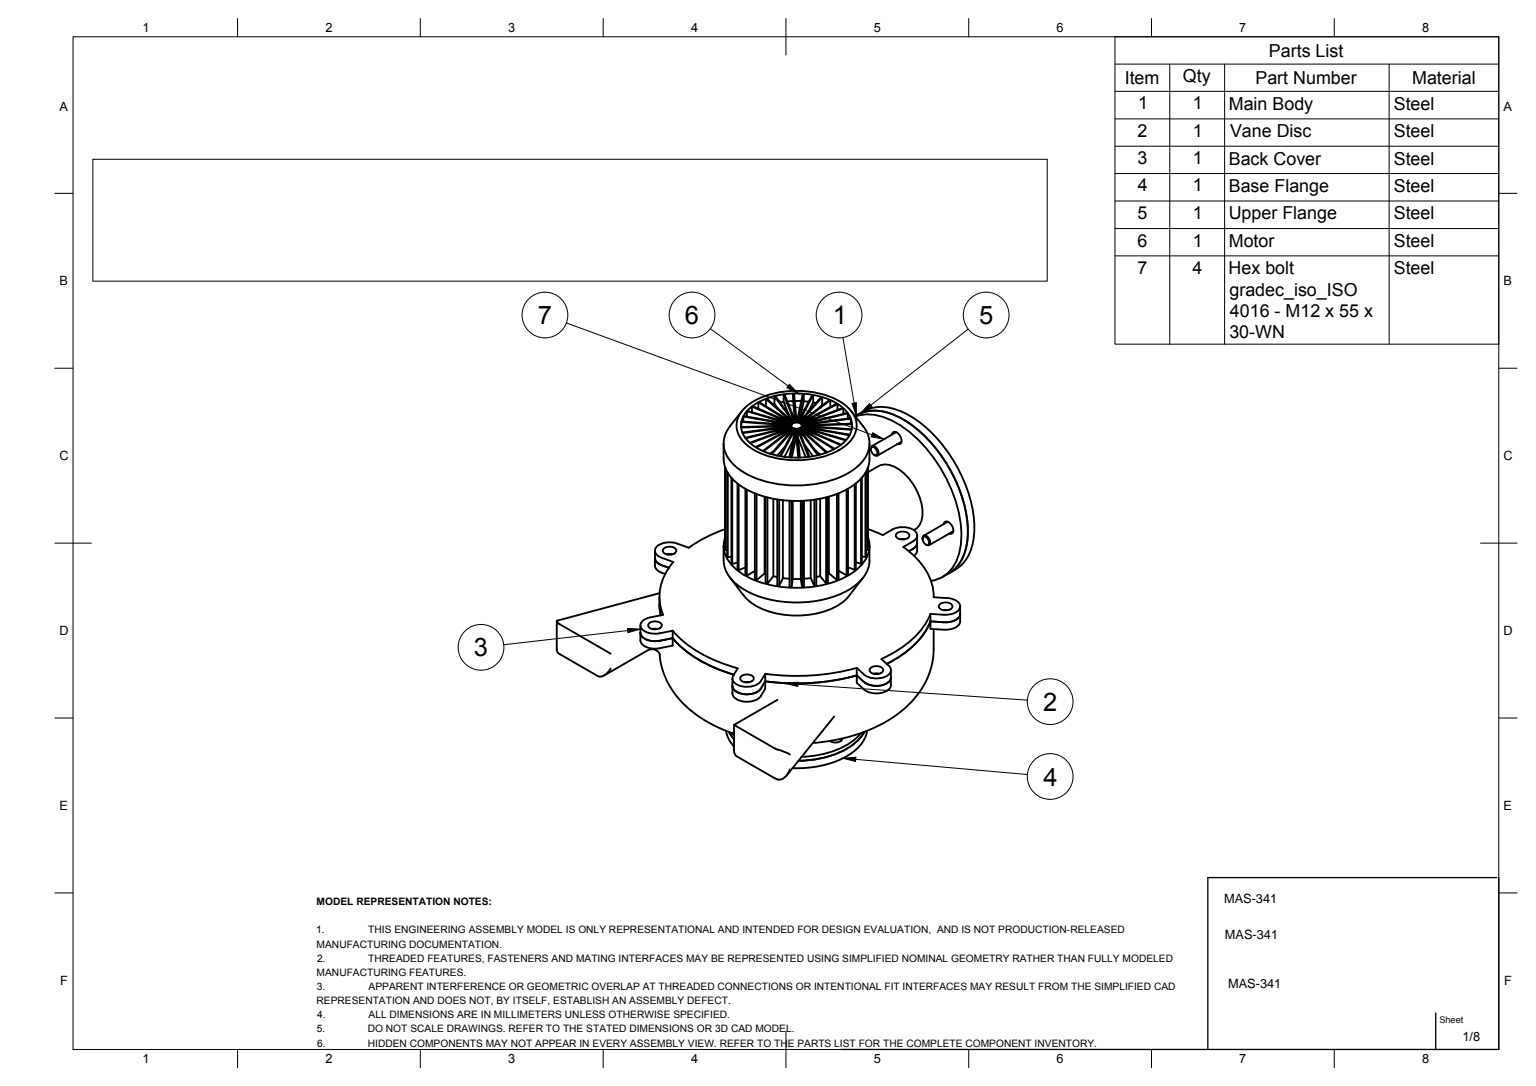
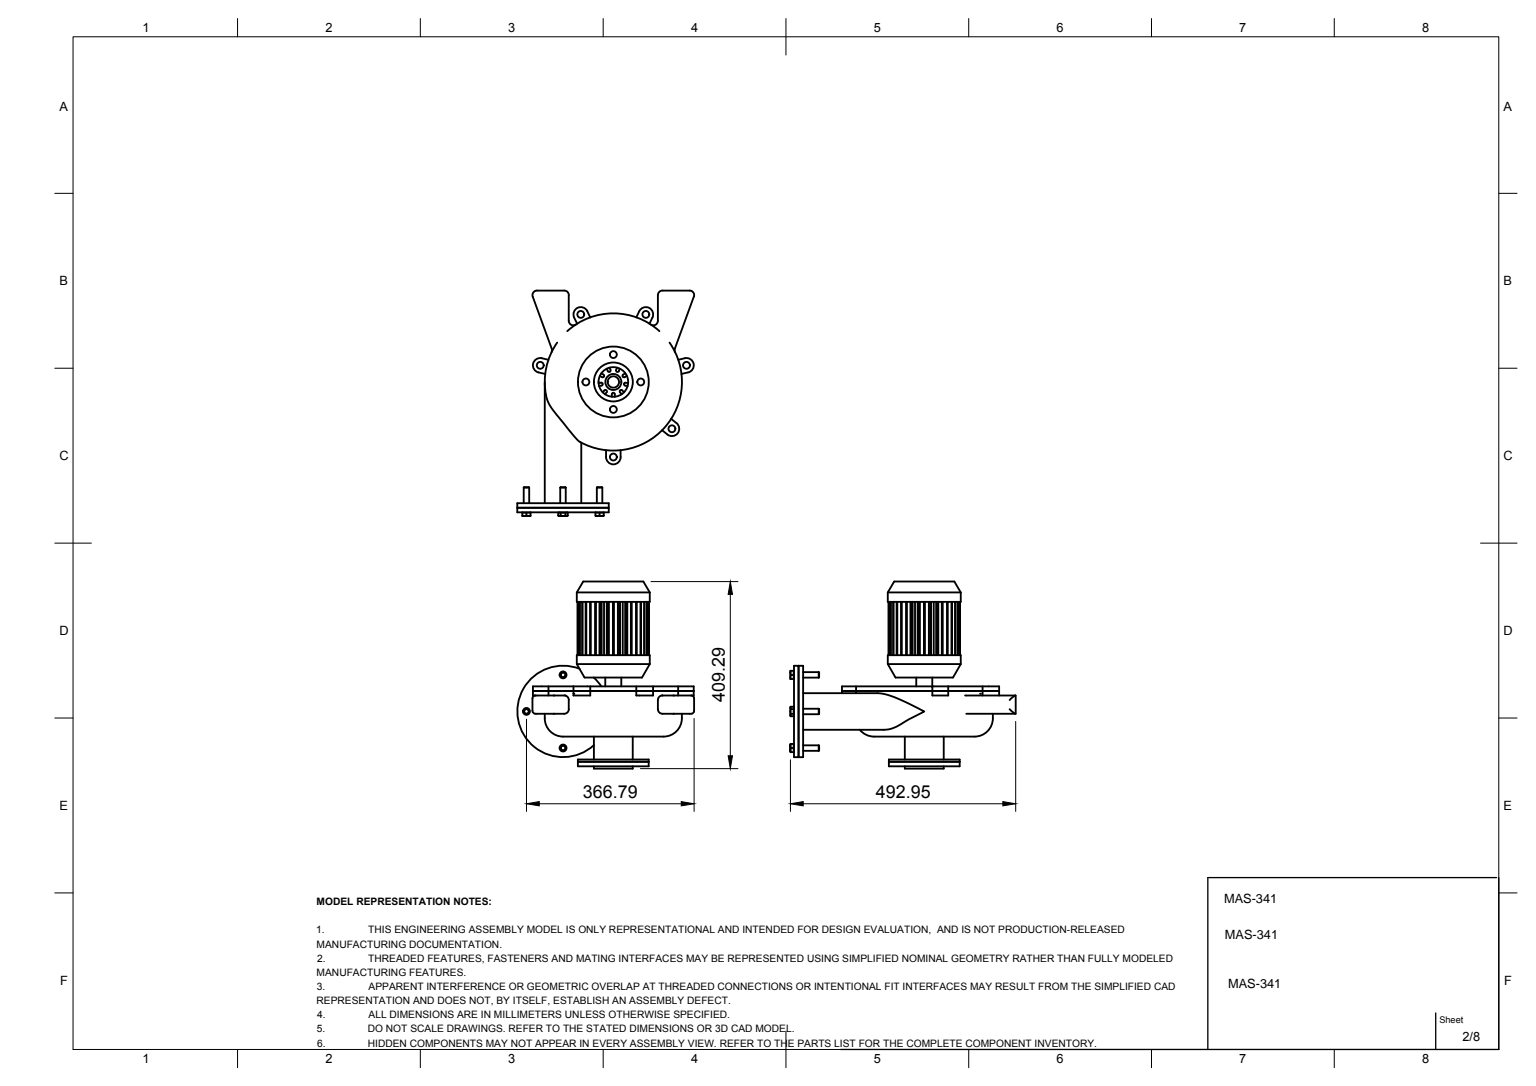
ISO-10303-21;
HEADER;
FILE_DESCRIPTION (('STEP AP214'),
    '1' );
FILE_NAME ('MAS-341',
    '2026-10-08T00:39:10',
    ( '' ),
    ( '' ),
    'SwSTEP 2.0',
    'SolidWorks 2025',
    '' );
FILE_SCHEMA (( 'AUTOMOTIVE_DESIGN' ));
ENDSEC;

DATA;
#1 = VERTEX_POINT ( 'NONE', #4469 ) ;
#2 = CARTESIAN_POINT ( 'NONE',  ( 97.60910239587762760, -133.8115172545202540, 8.514989709614523505 ) ) ;
#3 = DIRECTION ( 'NONE',  ( 0.000000000000000000, 0.000000000000000000, 1.000000000000000000 ) ) ;
#4 = PRODUCT ( 'Back Cover', 'Back Cover', '', ( #531 ) ) ;
#5 = EDGE_CURVE ( 'NONE', #5734, #13358, #17540, .T. ) ;
#6 = EDGE_CURVE ( 'NONE', #9325, #3604, #16957, .T. ) ;
#7 = DIRECTION ( 'NONE',  ( 0.000000000000000000, 0.000000000000000000, 1.000000000000000000 ) ) ;
#8 = AXIS2_PLACEMENT_3D ( 'NONE', #20241, #7754, #6443 ) ;
#9 = CARTESIAN_POINT ( 'NONE',  ( 0.000000000000000000, 0.000000000000000000, 49.99999999999999289 ) ) ;
#10 = VERTEX_POINT ( 'NONE', #9173 ) ;
#11 = LINE ( 'NONE', #3084, #15099 ) ;
#12 =( GEOMETRIC_REPRESENTATION_CONTEXT ( 3 ) GLOBAL_UNCERTAINTY_ASSIGNED_CONTEXT ( ( #1291 ) ) GLOBAL_UNIT_ASSIGNED_CONTEXT ( ( #18131, #16699, #13613 ) ) REPRESENTATION_CONTEXT ( 'NONE', 'WORKASPACE' ) );
#13 = DIRECTION ( 'NONE',  ( 1.000000000000000000, 0.000000000000000000, 0.000000000000000000 ) ) ;
#14 = CARTESIAN_POINT ( 'NONE',  ( 1.379293853801755176, -58.69016442926522359, 112.7772637782949943 ) ) ;
#15 = VECTOR ( 'NONE', #9741, 1000.000000000000000 ) ;
#16 = CARTESIAN_POINT ( 'NONE',  ( 95.93567628220807819, -116.0760901523964179, 30.45195958925782520 ) ) ;
#17 = VERTEX_POINT ( 'NONE', #1406 ) ;
#18 = LINE ( 'NONE', #19855, #18549 ) ;
#19 = CARTESIAN_POINT ( 'NONE',  ( -47.56244194535165803, -37.78198917157333625, 283.5832628385307999 ) ) ;
#20 = ORIENTED_EDGE ( 'NONE', *, *, #18426, .T. ) ;
#21 = ORIENTED_EDGE ( 'NONE', *, *, #3297, .T. ) ;
#22 = VERTEX_POINT ( 'NONE', #7636 ) ;
#23 = EDGE_CURVE ( 'NONE', #17780, #6819, #12333, .T. ) ;
#24 = DIRECTION ( 'NONE',  ( 1.000000000000000000, 0.000000000000000000, 0.000000000000000000 ) ) ;
#25 = ORIENTED_EDGE ( 'NONE', *, *, #13470, .F. ) ;
#26 = CARTESIAN_POINT ( 'NONE',  ( 78.68887634719571622, -147.8252249328912740, 39.99999999999999289 ) ) ;
#27 = FACE_BOUND ( 'NONE', #13868, .T. ) ;
#28 = ORIENTED_EDGE ( 'NONE', *, *, #7214, .F. ) ;
#29 = VECTOR ( 'NONE', #19093, 1000.000000000000000 ) ;
#30 = DIRECTION ( 'NONE',  ( 0.000000000000000000, 0.000000000000000000, 1.000000000000000000 ) ) ;
#31 = FACE_OUTER_BOUND ( 'NONE', #4493, .T. ) ;
#32 = CARTESIAN_POINT ( 'NONE',  ( 130.7934332354521132, -73.44669674648567081, 45.54261232719608188 ) ) ;
#33 = CARTESIAN_POINT ( 'NONE',  ( -84.44661573609343463, -123.9709896190455680, 39.82577217277482617 ) ) ;
#34 = EDGE_CURVE ( 'NONE', #17780, #13430, #14084, .T. ) ;
#35 = DIRECTION ( 'NONE',  ( -0.000000000000000000, -0.000000000000000000, 1.000000000000000000 ) ) ;
#36 = DIRECTION ( 'NONE',  ( 1.000000000000000000, 0.000000000000000000, 0.000000000000000000 ) ) ;
#37 = EDGE_CURVE ( 'NONE', #15836, #9172, #3251, .T. ) ;
#38 = CARTESIAN_POINT ( 'NONE',  ( -139.9569363493348249, 3.997132000652560802, 23.09995224052206453 ) ) ;
#39 = DIRECTION ( 'NONE',  ( 0.000000000000000000, 0.000000000000000000, 1.000000000000000000 ) ) ;
#40 = DIRECTION ( 'NONE',  ( -0.9396926207859104263, 0.3420201433256630508, 0.000000000000000000 ) ) ;
#41 = PLANE ( 'NONE',  #1345 ) ;
#42 = CARTESIAN_POINT ( 'NONE',  ( -133.8587666923834547, -78.85012038918891619, 37.00472930354037260 ) ) ;
#43 = ADVANCED_FACE ( 'NONE', ( #7739 ), #8149, .F. ) ;
#44 = ORIENTED_EDGE ( 'NONE', *, *, #7876, .F. ) ;
#45 = VECTOR ( 'NONE', #980, 1000.000000000000000 ) ;
#46 = DIRECTION ( 'NONE',  ( 0.000000000000000000, 1.000000000000000000, 0.000000000000000000 ) ) ;
#47 = AXIS2_PLACEMENT_3D ( 'NONE', #14477, #18892, #8730 ) ;
#48 = VERTEX_POINT ( 'NONE', #12848 ) ;
#49 = ORIENTED_EDGE ( 'NONE', *, *, #19031, .T. ) ;
#50 = ORIENTED_EDGE ( 'NONE', *, *, #6042, .F. ) ;
#51 = CARTESIAN_POINT ( 'NONE',  ( -144.9440567817290741, -14.18564734370175628, 2.776575249912347054 ) ) ;
#52 = CYLINDRICAL_SURFACE ( 'NONE', #15157, 62.91752772691707207 ) ;
#53 = CARTESIAN_POINT ( 'NONE',  ( 19.23677882349201695, -57.61823435390814296, 283.5832628385307999 ) ) ;
#54 = DIRECTION ( 'NONE',  ( -0.3747554100459959403, -0.9271237148521535021, 0.000000000000000000 ) ) ;
#55 = VERTEX_POINT ( 'NONE', #19106 ) ;
#56 = CARTESIAN_POINT ( 'NONE',  ( -95.11181282143326143, 95.73178764297979626, -26.71222966351301409 ) ) ;
#57 = CARTESIAN_POINT ( 'NONE',  ( -50.37374754117255549, -141.2886604036510221, 60.00000000000000000 ) ) ;
#58 = DIRECTION ( 'NONE',  ( -0.000000000000000000, -0.000000000000000000, -1.000000000000000000 ) ) ;
#59 = LINE ( 'NONE', #18583, #13084 ) ;
#60 = DIRECTION ( 'NONE',  ( -0.000000000000000000, -0.000000000000000000, 1.000000000000000000 ) ) ;
#61 = EDGE_CURVE ( 'NONE', #5572, #2811, #1813, .T. ) ;
#62 = ORIENTED_EDGE ( 'NONE', *, *, #6982, .T. ) ;
#63 = CARTESIAN_POINT ( 'NONE',  ( 134.0645693066686874, -77.56608579646832879, 36.26849213499117042 ) ) ;
#64 = CARTESIAN_POINT ( 'NONE',  ( -109.9999999999983515, 275.0000000000000000, 92.50000000000004263 ) ) ;
#65 = VERTEX_POINT ( 'NONE', #17476 ) ;
#66 = ORIENTED_EDGE ( 'NONE', *, *, #9551, .T. ) ;
#67 = ORIENTED_EDGE ( 'NONE', *, *, #294, .F. ) ;
#68 = ORIENTED_EDGE ( 'NONE', *, *, #8619, .T. ) ;
#69 = CARTESIAN_POINT ( 'NONE',  ( 57.41881860123199743, 83.27814316901175573, 14.88498244535504966 ) ) ;
#70 = VECTOR ( 'NONE', #7904, 1000.000000000000000 ) ;
#71 = ORIENTED_EDGE ( 'NONE', *, *, #11636, .F. ) ;
#72 = PLANE ( 'NONE',  #545 ) ;
#73 = DIRECTION ( 'NONE',  ( 1.000000000000000000, 0.000000000000000000, 0.000000000000000000 ) ) ;
#74 = DIRECTION ( 'NONE',  ( -0.000000000000000000, -0.000000000000000000, -1.000000000000000000 ) ) ;
#75 = LINE ( 'NONE', #4042, #2106 ) ;
#76 = CARTESIAN_POINT ( 'NONE',  ( 152.4599531637113330, -36.50981547336952104, 49.99999999999999289 ) ) ;
#77 = ORIENTED_EDGE ( 'NONE', *, *, #15533, .T. ) ;
#78 = DIRECTION ( 'NONE',  ( 0.4999999999999920619, -0.8660254037844431485, -3.488064225688951427E-15 ) ) ;
#79 = LINE ( 'NONE', #15635, #4891 ) ;
#80 = EDGE_LOOP ( 'NONE', ( #725, #12520, #18539, #7460 ) ) ;
#81 = UNCERTAINTY_MEASURE_WITH_UNIT (LENGTH_MEASURE( 1.000000000000000082E-05 ), #12072, 'distance_accuracy_value', 'NONE');
#82 = CARTESIAN_POINT ( 'NONE',  ( -82.22709333324932857, 122.5189358644918656, -23.80566512433226833 ) ) ;
#83 = CARTESIAN_POINT ( 'NONE',  ( -110.0000000000000142, 275.0000000000000000, 5.000000000000000888 ) ) ;
#84 = EDGE_CURVE ( 'NONE', #13974, #7495, #15567, .T. ) ;
#85 = CARTESIAN_POINT ( 'NONE',  ( 7.350000000000001421, 0.000000000000000000, 0.000000000000000000 ) ) ;
#86 = VECTOR ( 'NONE', #18456, 1000.000000000000000 ) ;
#87 = AXIS2_PLACEMENT_3D ( 'NONE', #5255, #2475, #14657 ) ;
#88 = LINE ( 'NONE', #6338, #12972 ) ;
#89 = CARTESIAN_POINT ( 'NONE',  ( 9.176097008933345123, -25.21111933077053990, 14.88498244535538895 ) ) ;
#90 = CARTESIAN_POINT ( 'NONE',  ( -56.84754764479025368, -154.7316448359455308, 49.99999999999999289 ) ) ;
#91 = ORIENTED_EDGE ( 'NONE', *, *, #10595, .F. ) ;
#92 = CARTESIAN_POINT ( 'NONE',  ( 128.2779226595531270, 102.2982297021113141, 60.00000000000000000 ) ) ;
#93 = VERTEX_POINT ( 'NONE', #12647 ) ;
#94 = VECTOR ( 'NONE', #4205, 1000.000000000000000 ) ;
#95 = ORIENTED_EDGE ( 'NONE', *, *, #17125, .F. ) ;
#96 = FACE_OUTER_BOUND ( 'NONE', #8145, .T. ) ;
#97 = EDGE_CURVE ( 'NONE', #13695, #10750, #5094, .T. ) ;
#98 = VERTEX_POINT ( 'NONE', #17267 ) ;
#99 = FACE_OUTER_BOUND ( 'NONE', #15672, .T. ) ;
#100 = FACE_BOUND ( 'NONE', #8738, .T. ) ;
#101 = ORIENTED_EDGE ( 'NONE', *, *, #14389, .F. ) ;
#102 = CARTESIAN_POINT ( 'NONE',  ( 100.3336596192663990, -130.0766330735003180, 3.023488127333376685 ) ) ;
#103 = CARTESIAN_POINT ( 'NONE',  ( 0.000000000000000000, 0.000000000000000000, 283.5832628385307999 ) ) ;
#104 = VECTOR ( 'NONE', #2637, 1000.000000000000000 ) ;
#105 = ADVANCED_FACE ( 'NONE', ( #15832 ), #1708, .T. ) ;
#106 = FACE_OUTER_BOUND ( 'NONE', #19908, .T. ) ;
#107 = SURFACE_SIDE_STYLE ('',( #15666 ) ) ;
#108 = VERTEX_POINT ( 'NONE', #3347 ) ;
#109 = CARTESIAN_POINT ( 'NONE',  ( 79.75827554147308263, 0.000000000000000000, 112.9440587442963562 ) ) ;
#110 = CYLINDRICAL_SURFACE ( 'NONE', #6774, 62.91752772691707207 ) ;
#111 = FACE_OUTER_BOUND ( 'NONE', #19672, .T. ) ;
#112 = CARTESIAN_POINT ( 'NONE',  ( 96.87131796860539623, -115.7364764686970489, 29.66028648393937317 ) ) ;
#113 = ORIENTED_EDGE ( 'NONE', *, *, #2779, .F. ) ;
#114 = DIRECTION ( 'NONE',  ( -3.129754055707530415E-16, 1.000000000000000000, 0.000000000000000000 ) ) ;
#115 = CARTESIAN_POINT ( 'NONE',  ( -70.46379820184749576, 132.4194400891323653, -1.343775461033565932 ) ) ;
#116 = AXIS2_PLACEMENT_3D ( 'NONE', #3572, #14207, #6645 ) ;
#117 = ORIENTED_EDGE ( 'NONE', *, *, #11334, .T. ) ;
#118 = EDGE_LOOP ( 'NONE', ( #19896, #4440, #15908, #1948 ) ) ;
#119 = ORIENTED_EDGE ( 'NONE', *, *, #13238, .T. ) ;
#120 =( NAMED_UNIT ( * ) SI_UNIT ( $, .STERADIAN. ) SOLID_ANGLE_UNIT ( ) );
#121 = EDGE_CURVE ( 'NONE', #7971, #3301, #6530, .T. ) ;
#122 = AXIS2_PLACEMENT_3D ( 'NONE', #14861, #16210, #14669 ) ;
#123 = EDGE_LOOP ( 'NONE', ( #19058, #8519, #18483, #4308 ) ) ;
#124 = ADVANCED_FACE ( 'NONE', ( #3050 ), #72, .T. ) ;
#125 = CARTESIAN_POINT ( 'NONE',  ( 28.06680738835026290, -53.87178215532764369, 293.5832628385307999 ) ) ;
#126 = LINE ( 'NONE', #5341, #13935 ) ;
#127 = VECTOR ( 'NONE', #6121, 1000.000000000000000 ) ;
#128 = ORIENTED_EDGE ( 'NONE', *, *, #9739, .T. ) ;
#129 = FACE_OUTER_BOUND ( 'NONE', #6146, .T. ) ;
#130 = DIRECTION ( 'NONE',  ( 0.000000000000000000, 1.000000000000000000, 0.000000000000000000 ) ) ;
#131 = DIRECTION ( 'NONE',  ( -0.1736481776669408228, -0.9848077530122062440, 2.152196535136390085E-15 ) ) ;
#132 = CARTESIAN_POINT ( 'NONE',  ( -95.59344839194261567, -116.1516065318577233, 31.25619608454541165 ) ) ;
#133 = LINE ( 'NONE', #6488, #17538 ) ;
#134 = CARTESIAN_POINT ( 'NONE',  ( -140.0000000000000284, 1.714505518806295230E-14, 23.02775637731986436 ) ) ;
#135 = EDGE_CURVE ( 'NONE', #17975, #14483, #10909, .T. ) ;
#136 = CARTESIAN_POINT ( 'NONE',  ( 141.8714406926368099, -48.70825716237082759, 49.99999999999999289 ) ) ;
#137 = VECTOR ( 'NONE', #8001, 1000.000000000000000 ) ;
#138 = CARTESIAN_POINT ( 'NONE',  ( -19.79297637435821500, 18.57624240429758800, 39.88498244535558968 ) ) ;
#139 = PLANE ( 'NONE',  #10813 ) ;
#140 = CARTESIAN_POINT ( 'NONE',  ( -123.8565975624213849, -84.62454961663081576, 40.61527585688936881 ) ) ;
#141 = VERTEX_POINT ( 'NONE', #14296 ) ;
#142 = DIRECTION ( 'NONE',  ( -0.000000000000000000, -0.000000000000000000, 1.000000000000000000 ) ) ;
#143 = CIRCLE ( 'NONE', #11572, 77.50000000000000000 ) ;
#144 = ORIENTED_EDGE ( 'NONE', *, *, #11299, .F. ) ;
#145 = EDGE_CURVE ( 'NONE', #10155, #5152, #9485, .T. ) ;
#146 = ADVANCED_FACE ( 'NONE', ( #6627 ), #17167, .F. ) ;
#147 = EDGE_LOOP ( 'NONE', ( #10880, #3979, #3844, #3785, #18936 ) ) ;
#148 = ADVANCED_FACE ( 'NONE', ( #7839 ), #6224, .F. ) ;
#149 = EDGE_CURVE ( 'NONE', #12149, #16123, #12294, .T. ) ;
#150 = ORIENTED_EDGE ( 'NONE', *, *, #14501, .F. ) ;
#151 = AXIS2_PLACEMENT_3D ( 'NONE', #5744, #3184, #10529 ) ;
#152 = CARTESIAN_POINT ( 'NONE',  ( -144.3459975433503359, -14.90824844061875432, 11.80575795572019437 ) ) ;
#153 = DIRECTION ( 'NONE',  ( 0.000000000000000000, 0.000000000000000000, -1.000000000000000000 ) ) ;
#154 = LINE ( 'NONE', #15601, #13008 ) ;
#155 = DIRECTION ( 'NONE',  ( 0.000000000000000000, 0.000000000000000000, 1.000000000000000000 ) ) ;
#156 = CARTESIAN_POINT ( 'NONE',  ( -77.50000000000000000, 9.491012693391988181E-15, -105.0000000000000142 ) ) ;
#157 = EDGE_CURVE ( 'NONE', #11944, #5361, #6437, .T. ) ;
#158 = LINE ( 'NONE', #9470, #15417 ) ;
#159 = DIRECTION ( 'NONE',  ( -0.000000000000000000, -0.000000000000000000, 1.000000000000000000 ) ) ;
#160 = CARTESIAN_POINT ( 'NONE',  ( 104.3997176008718668, -123.8500140569468897, 39.51069475786240304 ) ) ;
#161 = AXIS2_PLACEMENT_3D ( 'NONE', #19945, #4400, #6050 ) ;
#162 = CARTESIAN_POINT ( 'NONE',  ( 0.000000000000000000, 0.000000000000000000, 283.5832628385307999 ) ) ;
#163 = ORIENTED_EDGE ( 'NONE', *, *, #16525, .F. ) ;
#164 = CARTESIAN_POINT ( 'NONE',  ( 131.4393841463105730, -72.38802639019482399, 37.47509838629414247 ) ) ;
#165 = CARTESIAN_POINT ( 'NONE',  ( -97.49999999999997158, -195.8578643762690206, 4.142135623730952787 ) ) ;
#166 = VERTEX_POINT ( 'NONE', #19011 ) ;
#167 = ORIENTED_EDGE ( 'NONE', *, *, #19754, .F. ) ;
#168 = EDGE_CURVE ( 'NONE', #13542, #6667, #19206, .T. ) ;
#169 = ORIENTED_EDGE ( 'NONE', *, *, #10850, .T. ) ;
#170 = LINE ( 'NONE', #6528, #17757 ) ;
#171 = ORIENTED_EDGE ( 'NONE', *, *, #16914, .T. ) ;
#172 = CARTESIAN_POINT ( 'NONE',  ( 51.23821591265094355, 28.63313560863489471, 132.4711112102474146 ) ) ;
#173 = VECTOR ( 'NONE', #8479, 1000.000000000000000 ) ;
#174 = EDGE_CURVE ( 'NONE', #2962, #5478, #10345, .T. ) ;
#175 = DIRECTION ( 'NONE',  ( -0.000000000000000000, -0.000000000000000000, 1.000000000000000000 ) ) ;
#176 = FACE_BOUND ( 'NONE', #16626, .T. ) ;
#177 = CARTESIAN_POINT ( 'NONE',  ( 44.79940644582654841, -41.02350267428983699, 293.5832628385307999 ) ) ;
#178 = CARTESIAN_POINT ( 'NONE',  ( -85.53020504959707182, -140.9188050298390067, 49.99999999999999289 ) ) ;
#179 = ORIENTED_EDGE ( 'NONE', *, *, #8168, .F. ) ;
#180 = CARTESIAN_POINT ( 'NONE',  ( 125.6254798881099362, -81.96796683352708612, -9.529669441935290308 ) ) ;
#181 = CARTESIAN_POINT ( 'NONE',  ( -57.92514141135452377, -18.28503710798565152, 293.5832628385307999 ) ) ;
#182 = VERTEX_POINT ( 'NONE', #8245 ) ;
#183 = DIRECTION ( 'NONE',  ( -0.000000000000000000, -1.000000000000000000, -0.000000000000000000 ) ) ;
#184 = DIRECTION ( 'NONE',  ( -0.000000000000000000, -0.000000000000000000, 1.000000000000000000 ) ) ;
#185 = VECTOR ( 'NONE', #17338, 999.9999999999998863 ) ;
#186 = DIRECTION ( 'NONE',  ( 0.4999999999999978906, 0.8660254037844397068, 0.000000000000000000 ) ) ;
#187 = CYLINDRICAL_SURFACE ( 'NONE', #11980, 150.0000000000000284 ) ;
#188 =( GEOMETRIC_REPRESENTATION_CONTEXT ( 3 ) GLOBAL_UNCERTAINTY_ASSIGNED_CONTEXT ( ( #9055 ) ) GLOBAL_UNIT_ASSIGNED_CONTEXT ( ( #6659, #405, #9614 ) ) REPRESENTATION_CONTEXT ( 'NONE', 'WORKASPACE' ) );
#189 = CARTESIAN_POINT ( 'NONE',  ( 89.20186311087663000, -120.5960167300875980, 45.74363724982469392 ) ) ;
#190 = ORIENTED_EDGE ( 'NONE', *, *, #18942, .F. ) ;
#191 = CARTESIAN_POINT ( 'NONE',  ( -7.500000000000006217, 164.0736214083062805, 49.99999999999999289 ) ) ;
#192 = ORIENTED_EDGE ( 'NONE', *, *, #7035, .T. ) ;
#193 = ORIENTED_EDGE ( 'NONE', *, *, #1304, .F. ) ;
#194 = DIRECTION ( 'NONE',  ( 0.000000000000000000, 0.000000000000000000, -1.000000000000000000 ) ) ;
#195 = VERTEX_POINT ( 'NONE', #2590 ) ;
#196 = VECTOR ( 'NONE', #6508, 1000.000000000000000 ) ;
#197 = DIRECTION ( 'NONE',  ( -0.000000000000000000, -0.000000000000000000, 1.000000000000000000 ) ) ;
#198 = CARTESIAN_POINT ( 'NONE',  ( 25.99419088092191643, -73.82206860051539365, 248.9926560891072143 ) ) ;
#199 = EDGE_LOOP ( 'NONE', ( #8551, #11635, #6168 ) ) ;
#200 = DIRECTION ( 'NONE',  ( 0.000000000000000000, 0.000000000000000000, 1.000000000000000000 ) ) ;
#201 = DIRECTION ( 'NONE',  ( -0.000000000000000000, -0.000000000000000000, 1.000000000000000000 ) ) ;
#202 = DIRECTION ( 'NONE',  ( -0.6427876096865458022, 0.7660444431189726844, 0.000000000000000000 ) ) ;
#203 = LINE ( 'NONE', #14432, #8189 ) ;
#204 = DIRECTION ( 'NONE',  ( -1.000000000000000000, -0.000000000000000000, -0.000000000000000000 ) ) ;
#205 = ORIENTED_EDGE ( 'NONE', *, *, #13470, .T. ) ;
#206 = LINE ( 'NONE', #17312, #2056 ) ;
#207 = FACE_OUTER_BOUND ( 'NONE', #7256, .T. ) ;
#208 = DIRECTION ( 'NONE',  ( 1.000000000000000000, 0.000000000000000000, 0.000000000000000000 ) ) ;
#209 = LINE ( 'NONE', #17715, #417 ) ;
#210 = ORIENTED_EDGE ( 'NONE', *, *, #884, .F. ) ;
#211 = VECTOR ( 'NONE', #4896, 1000.000000000000114 ) ;
#212 = FACE_OUTER_BOUND ( 'NONE', #80, .T. ) ;
#213 = CARTESIAN_POINT ( 'NONE',  ( -71.48370871149657546, 131.8717905529093173, 15.83076793550482542 ) ) ;
#214 = ORIENTED_EDGE ( 'NONE', *, *, #634, .F. ) ;
#215 = ORIENTED_EDGE ( 'NONE', *, *, #14623, .F. ) ;
#217 = ORIENTED_EDGE ( 'NONE', *, *, #13252, .T. ) ;
#216 = VECTOR ( 'NONE', #7323, 999.9999999999998863 ) ;
#218 = DIRECTION ( 'NONE',  ( 0.000000000000000000, 0.000000000000000000, 1.000000000000000000 ) ) ;
#219 = VERTEX_POINT ( 'NONE', #7381 ) ;
#220 = EDGE_CURVE ( 'NONE', #5955, #14128, #18233, .T. ) ;
#221 = LINE ( 'NONE', #125, #3582 ) ;
#222 = CARTESIAN_POINT ( 'NONE',  ( -139.5020293846663435, 55.14116363050599290, 32.01918336342640004 ) ) ;
#223 = ORIENTED_EDGE ( 'NONE', *, *, #17123, .T. ) ;
#224 = FACE_OUTER_BOUND ( 'NONE', #2485, .T. ) ;
#225 = LINE ( 'NONE', #20072, #5672 ) ;
#226 = CARTESIAN_POINT ( 'NONE',  ( 134.9252074077220129, -65.53799637400003064, 33.62285034463288724 ) ) ;
#227 = CIRCLE ( 'NONE', #11655, 3.224098631618461663 ) ;
#228 = CARTESIAN_POINT ( 'NONE',  ( -96.81625497257122959, -114.6298681929799557, 36.57121525224014391 ) ) ;
#229 = FACE_OUTER_BOUND ( 'NONE', #16622, .T. ) ;
#230 = CARTESIAN_POINT ( 'NONE',  ( -90.17913298585699522, -119.8669913176027961, -6.508363994189858559 ) ) ;
#231 = DIRECTION ( 'NONE',  ( 0.000000000000000000, 0.000000000000000000, 1.000000000000000000 ) ) ;
#232 = DIRECTION ( 'NONE',  ( 1.000000000000000000, 0.000000000000000000, 0.000000000000000000 ) ) ;
#233 = CIRCLE ( 'NONE', #865, 60.74260934110282051 ) ;
#234 = EDGE_CURVE ( 'NONE', #6701, #18758, #15059, .T. ) ;
#235 = DIRECTION ( 'NONE',  ( 6.982962677686266711E-15, -0.000000000000000000, 1.000000000000000000 ) ) ;
#236 = VECTOR ( 'NONE', #1051, 1000.000000000000000 ) ;
#237 = EDGE_CURVE ( 'NONE', #5955, #1847, #14266, .T. ) ;
#238 = PLANE ( 'NONE',  #10473 ) ;
#239 = CARTESIAN_POINT ( 'NONE',  ( 23.23469325536214214, -13.41455640552199924, 14.88498244535528947 ) ) ;
#240 = CARTESIAN_POINT ( 'NONE',  ( -133.3512892972259749, -81.69145041113908690, 38.21234876929968038 ) ) ;
#241 = VERTEX_POINT ( 'NONE', #4112 ) ;
#242 = EDGE_CURVE ( 'NONE', #7766, #5287, #5764, .T. ) ;
#243 = CARTESIAN_POINT ( 'NONE',  ( -55.43188410062182925, -19.30071112029661151, 248.9926560891072143 ) ) ;
#244 = VERTEX_POINT ( 'NONE', #16407 ) ;
#245 = AXIS2_PLACEMENT_3D ( 'NONE', #14497, #6431, #6630 ) ;
#246 = ORIENTED_EDGE ( 'NONE', *, *, #6218, .F. ) ;
#247 = EDGE_CURVE ( 'NONE', #18829, #4599, #4215, .T. ) ;
#248 = CIRCLE ( 'NONE', #6127, 15.91767397667354800 ) ;
#249 = AXIS2_PLACEMENT_3D ( 'NONE', #15715, #7622, #7927 ) ;
#250 = ORIENTED_EDGE ( 'NONE', *, *, #6281, .T. ) ;
#251 = CARTESIAN_POINT ( 'NONE',  ( -142.2837698990419710, -17.71062413665211466, 18.52607103759555685 ) ) ;
#252 = CARTESIAN_POINT ( 'NONE',  ( 0.000000000000000000, 0.000000000000000000, 293.5832628385307999 ) ) ;
#253 = CARTESIAN_POINT ( 'NONE',  ( -3.911853314815645799, 4.196299268919075232, 293.5832628385307999 ) ) ;
#254 = CARTESIAN_POINT ( 'NONE',  ( 15.91767397667354800, 164.0736214083062805, 49.99999999999999289 ) ) ;
#255 = DIRECTION ( 'NONE',  ( 1.000000000000000000, 0.000000000000000000, 0.000000000000000000 ) ) ;
#256 = DIRECTION ( 'NONE',  ( -0.000000000000000000, -0.000000000000000000, 1.000000000000000000 ) ) ;
#257 = FACE_OUTER_BOUND ( 'NONE', #10692, .T. ) ;
#258 = EDGE_CURVE ( 'NONE', #16031, #14304, #11946, .T. ) ;
#259 = PLANE ( 'NONE',  #6247 ) ;
#260 = FACE_OUTER_BOUND ( 'NONE', #11432, .T. ) ;
#261 = AXIS2_PLACEMENT_3D ( 'NONE', #5388, #13050, #3942 ) ;
#262 = EDGE_CURVE ( 'NONE', #18721, #13125, #19565, .T. ) ;
#263 = ORIENTED_EDGE ( 'NONE', *, *, #10525, .T. ) ;
#264 = AXIS2_PLACEMENT_3D ( 'NONE', #15615, #1602, #16694 ) ;
#265 = CARTESIAN_POINT ( 'NONE',  ( 134.2531151303012109, -76.34772591579755385, 35.47645838411665409 ) ) ;
#266 = CARTESIAN_POINT ( 'NONE',  ( 132.1955596402976596, -87.17962382538661359, 39.63083459970911804 ) ) ;
#267 = ORIENTED_EDGE ( 'NONE', *, *, #4626, .T. ) ;
#268 = ORIENTED_EDGE ( 'NONE', *, *, #10367, .T. ) ;
#269 = VERTEX_POINT ( 'NONE', #14956 ) ;
#270 = VERTEX_POINT ( 'NONE', #10443 ) ;
#271 = DIRECTION ( 'NONE',  ( -0.9511061040868794558, -0.3088643371590157338, 0.000000000000000000 ) ) ;
#272 = EDGE_CURVE ( 'NONE', #301, #10908, #19490, .T. ) ;
#273 = VECTOR ( 'NONE', #15752, 1000.000000000000000 ) ;
#274 = VERTEX_POINT ( 'NONE', #2392 ) ;
#275 = DIRECTION ( 'NONE',  ( 1.000000000000000000, 0.000000000000000000, -0.000000000000000000 ) ) ;
#276 = VECTOR ( 'NONE', #14469, 1000.000000000000000 ) ;
#277 = FACE_OUTER_BOUND ( 'NONE', #4264, .T. ) ;
#278 = CIRCLE ( 'NONE', #5508, 7.500000000000020428 ) ;
#279 = PLANE ( 'NONE',  #19707 ) ;
#280 = CARTESIAN_POINT ( 'NONE',  ( 57.61823435390807902, 19.23677882349220880, 293.5832628385307999 ) ) ;
#281 = ORIENTED_EDGE ( 'NONE', *, *, #5638, .F. ) ;
#282 = DIRECTION ( 'NONE',  ( 4.650550193362991910E-16, 1.000000000000000000, 0.000000000000000000 ) ) ;
#283 = DIRECTION ( 'NONE',  ( 6.982962677686266711E-15, -0.000000000000000000, 1.000000000000000000 ) ) ;
#284 = ORIENTED_EDGE ( 'NONE', *, *, #8836, .T. ) ;
#285 = CARTESIAN_POINT ( 'NONE',  ( -0.8220851292435327196, -62.91215678473957240, 132.4711112102474146 ) ) ;
#286 = DIRECTION ( 'NONE',  ( -0.8660254037844345998, -0.5000000000000069944, 0.000000000000000000 ) ) ;
#287 = EDGE_CURVE ( 'NONE', #13667, #5147, #20127, .T. ) ;
#288 = CARTESIAN_POINT ( 'NONE',  ( 62.09913334491125170, 10.11498556985180208, 132.4711112102474146 ) ) ;
#289 = LINE ( 'NONE', #19024, #1463 ) ;
#290 = CARTESIAN_POINT ( 'NONE',  ( 55.43188410062170135, 19.30071112029698455, 248.9926560891072143 ) ) ;
#291 = DIRECTION ( 'NONE',  ( -1.000000000000000000, 0.000000000000000000, 0.000000000000000000 ) ) ;
#292 = FACE_OUTER_BOUND ( 'NONE', #9039, .T. ) ;
#293 = AXIS2_PLACEMENT_3D ( 'NONE', #9235, #1570, #18553 ) ;
#294 = EDGE_CURVE ( 'NONE', #11013, #2211, #842, .T. ) ;
#295 = VERTEX_POINT ( 'NONE', #16702 ) ;
#296 = VECTOR ( 'NONE', #6808, 1000.000000000000114 ) ;
#297 = DIRECTION ( 'NONE',  ( 1.000000000000000000, 0.000000000000000000, 0.000000000000000000 ) ) ;
#298 = ORIENTED_EDGE ( 'NONE', *, *, #10704, .T. ) ;
#299 = ORIENTED_EDGE ( 'NONE', *, *, #9841, .T. ) ;
#300 = LINE ( 'NONE', #15954, #4521 ) ;
#301 = VERTEX_POINT ( 'NONE', #13513 ) ;
#302 = CIRCLE ( 'NONE', #17951, 3.224098631618462552 ) ;
#303 = CARTESIAN_POINT ( 'NONE',  ( 15.91767397667354800, 164.0736214083062805, 39.99999999999999289 ) ) ;
#304 = FACE_BOUND ( 'NONE', #20117, .T. ) ;
#305 = EDGE_LOOP ( 'NONE', ( #2327, #8715, #1443, #6118 ) ) ;
#306 = LINE ( 'NONE', #12370, #13574 ) ;
#307 = AXIS2_PLACEMENT_3D ( 'NONE', #2543, #16563, #13781 ) ;
#308 = CARTESIAN_POINT ( 'NONE',  ( -109.9999999999983515, 275.0000000000000000, 92.50000000000004263 ) ) ;
#309 = CARTESIAN_POINT ( 'NONE',  ( -97.49999999999997158, -190.0000000000000000, 10.00000000000000178 ) ) ;
#310 = ORIENTED_EDGE ( 'NONE', *, *, #14972, .F. ) ;
#311 = LINE ( 'NONE', #12579, #10853 ) ;
#312 = CARTESIAN_POINT ( 'NONE',  ( 57.61823435390807902, 19.23677882349220880, 293.5832628385307999 ) ) ;
#313 = FACE_OUTER_BOUND ( 'NONE', #5653, .T. ) ;
#314 = CARTESIAN_POINT ( 'NONE',  ( 106.3852469178137170, -120.5001569748608432, 39.95380131650621536 ) ) ;
#315 = VERTEX_POINT ( 'NONE', #3550 ) ;
#316 = DIRECTION ( 'NONE',  ( -1.000000000000000000, 0.000000000000000000, 6.976128451377902853E-15 ) ) ;
#317 = CARTESIAN_POINT ( 'NONE',  ( -85.08865936083807924, 123.5409191676841374, 36.33575822748944972 ) ) ;
#318 = EDGE_LOOP ( 'NONE', ( #10849, #15517, #10410, #10745 ) ) ;
#319 = AXIS2_PLACEMENT_3D ( 'NONE', #17195, #12465, #6453 ) ;
#320 = VECTOR ( 'NONE', #3029, 1000.000000000000000 ) ;
#321 = VERTEX_POINT ( 'NONE', #7094 ) ;
#322 = EDGE_LOOP ( 'NONE', ( #19155, #18434, #14933, #18302 ) ) ;
#323 = SHAPE_DEFINITION_REPRESENTATION ( #15864, #15821 ) ;
#324 = ORIENTED_EDGE ( 'NONE', *, *, #14683, .T. ) ;
#325 = CARTESIAN_POINT ( 'NONE',  ( -19.23614321207235278, 57.61627707419557964, 283.5832628385307999 ) ) ;
#326 = CARTESIAN_POINT ( 'NONE',  ( -149.9999999999999716, 1.115331095350416746, 5.575954458838749517 ) ) ;
#327 = ORIENTED_EDGE ( 'NONE', *, *, #9501, .F. ) ;
#328 = CARTESIAN_POINT ( 'NONE',  ( 85.53020504959901871, -140.9188050298377846, 60.00000000000000000 ) ) ;
#329 = DIRECTION ( 'NONE',  ( -0.3420201433256601087, -0.9396926207859114255, 0.000000000000000000 ) ) ;
#330 = CARTESIAN_POINT ( 'NONE',  ( 132.6585078626522716, -70.01400725886476550, 42.31265725997803884 ) ) ;
#331 = VECTOR ( 'NONE', #5545, 1000.000000000000000 ) ;
#332 = CIRCLE ( 'NONE', #12417, 60.74260934110282051 ) ;
#333 = CARTESIAN_POINT ( 'NONE',  ( -89.20186311087657316, -120.5960167300876407, -5.743637249824701918 ) ) ;
#334 = CARTESIAN_POINT ( 'NONE',  ( 113.3640620605769413, -25.59923667990641150, 14.88498244535466064 ) ) ;
#335 = DIRECTION ( 'NONE',  ( -0.000000000000000000, -0.000000000000000000, 1.000000000000000000 ) ) ;
#336 = DIRECTION ( 'NONE',  ( -0.000000000000000000, -0.000000000000000000, 1.000000000000000000 ) ) ;
#337 = LINE ( 'NONE', #14255, #1684 ) ;
#338 = DIRECTION ( 'NONE',  ( 1.000000000000000000, 0.000000000000000000, 0.000000000000000000 ) ) ;
#339 = FACE_OUTER_BOUND ( 'NONE', #16289, .T. ) ;
#340 = EDGE_CURVE ( 'NONE', #18152, #7860, #943, .T. ) ;
#341 = ORIENTED_EDGE ( 'NONE', *, *, #8132, .T. ) ;
#342 = DIRECTION ( 'NONE',  ( -0.000000000000000000, -0.000000000000000000, 1.000000000000000000 ) ) ;
#343 = ORIENTED_EDGE ( 'NONE', *, *, #631, .F. ) ;
#344 = VECTOR ( 'NONE', #11455, 1000.000000000000000 ) ;
#345 = VERTEX_POINT ( 'NONE', #11779 ) ;
#346 = EDGE_CURVE ( 'NONE', #17320, #3067, #19461, .T. ) ;
#347 = VERTEX_POINT ( 'NONE', #3651 ) ;
#348 = EDGE_CURVE ( 'NONE', #14755, #3199, #18041, .T. ) ;
#349 = CARTESIAN_POINT ( 'NONE',  ( 0.000000000000000000, -7.794228634059948035, -4.499999999999999112 ) ) ;
#350 = LINE ( 'NONE', #4765, #14650 ) ;
#351 = DIRECTION ( 'NONE',  ( -0.000000000000000000, -0.000000000000000000, 1.000000000000000000 ) ) ;
#352 = ORIENTED_EDGE ( 'NONE', *, *, #1999, .T. ) ;
#353 = CARTESIAN_POINT ( 'NONE',  ( -29.99999999999887379, 265.0000000000000000, 12.49999999999916511 ) ) ;
#354 = CIRCLE ( 'NONE', #18993, 3.224098631618460331 ) ;
#355 = CARTESIAN_POINT ( 'NONE',  ( 68.18670162478805707, 38.41834839689404646, 248.9926560891072143 ) ) ;
#356 = FACE_OUTER_BOUND ( 'NONE', #14079, .T. ) ;
#357 = CARTESIAN_POINT ( 'NONE',  ( 44.79787735033391272, -41.02212542604626577, 293.5832628385307999 ) ) ;
#358 = AXIS2_PLACEMENT_3D ( 'NONE', #19876, #8929, #1155 ) ;
#359 = CARTESIAN_POINT ( 'NONE',  ( 0.000000000000000000, 0.000000000000000000, -110.0000000000000000 ) ) ;
#360 = EDGE_CURVE ( 'NONE', #2215, #19198, #19663, .T. ) ;
#361 = ORIENTED_EDGE ( 'NONE', *, *, #7399, .T. ) ;
#362 = DIRECTION ( 'NONE',  ( 6.982962677686266711E-15, -0.000000000000000000, 1.000000000000000000 ) ) ;
#363 = DIRECTION ( 'NONE',  ( -0.9511061040868794558, -0.3088643371590157338, 0.000000000000000000 ) ) ;
#364 = ORIENTED_EDGE ( 'NONE', *, *, #5614, .T. ) ;
#365 = CIRCLE ( 'NONE', #11782, 77.50000000000000000 ) ;
#366 = ORIENTED_EDGE ( 'NONE', *, *, #2785, .T. ) ;
#367 = EDGE_LOOP ( 'NONE', ( #4657, #4676 ) ) ;
#368 = ORIENTED_EDGE ( 'NONE', *, *, #19103, .F. ) ;
#369 = VECTOR ( 'NONE', #15962, 1000.000000000000000 ) ;
#370 = EDGE_CURVE ( 'NONE', #6318, #12537, #20174, .T. ) ;
#371 = VERTEX_POINT ( 'NONE', #9014 ) ;
#372 = DIRECTION ( 'NONE',  ( -0.000000000000000000, -0.000000000000000000, -1.000000000000000000 ) ) ;
#373 = ADVANCED_FACE ( 'NONE', ( #2893 ), #13929, .F. ) ;
#374 = AXIS2_PLACEMENT_3D ( 'NONE', #8108, #8211, #6887 ) ;
#375 = B_SPLINE_CURVE_WITH_KNOTS ( 'NONE', 3,
 ( #12809, #14142, #6181, #4742, #226, #1768, #17536, #3410, #17117, #330, #12398, #9642, #6588, #32, #9545, #19072, #8099, #14247, #3103, #15890, #18860, #4637, #17333, #1869 ),
 .UNSPECIFIED., .F., .F.,
 ( 4, 2, 2, 2, 2, 2, 2, 2, 2, 2, 2, 4 ),
 ( 0.000000000000000000, 0.002185557465519395465, 0.004371114931038790931, 0.008742229862077573188, 0.01311334479311635458, 0.01529890225863574441, 0.01748445972415513250, 0.02185557465519396420, 0.02404113212071339739, 0.02622668958623283059, 0.03059780451727174902, 0.03496891944831063970 ),
 .UNSPECIFIED. ) ;
#376 = EDGE_CURVE ( 'NONE', #12874, #17522, #10545, .T. ) ;
#377 = CARTESIAN_POINT ( 'NONE',  ( 0.000000000000000000, 0.000000000000000000, 49.99999999999999289 ) ) ;
#378 = DIRECTION ( 'NONE',  ( -0.000000000000000000, -1.000000000000000000, -0.000000000000000000 ) ) ;
#379 = DIRECTION ( 'NONE',  ( -6.982962677686266711E-15, 0.000000000000000000, -1.000000000000000000 ) ) ;
#380 = VERTEX_POINT ( 'NONE', #4526 ) ;
#381 = CARTESIAN_POINT ( 'NONE',  ( 133.7324673749508577, -67.93981414779143790, 0.4927691020655204368 ) ) ;
#382 = CARTESIAN_POINT ( 'NONE',  ( -61.81362617575094021, 11.73417718768112294, 132.4711112102474146 ) ) ;
#383 = VERTEX_POINT ( 'NONE', #14037 ) ;
#384 = CARTESIAN_POINT ( 'NONE',  ( 54.07248341783252954, -32.16802499836759921, 293.5832628385307999 ) ) ;
#385 = CARTESIAN_POINT ( 'NONE',  ( 0.000000000000000000, 0.000000000000000000, 112.9440587442963562 ) ) ;
#386 = DIRECTION ( 'NONE',  ( 1.000000000000000000, 0.000000000000000000, 0.000000000000000000 ) ) ;
#387 = CARTESIAN_POINT ( 'NONE',  ( -109.9999999999983515, 285.0000000000000568, 92.50000000000004263 ) ) ;
#388 = EDGE_CURVE ( 'NONE', #16701, #14351, #10960, .T. ) ;
#389 = DIRECTION ( 'NONE',  ( -1.000000000000000000, 0.000000000000000000, 0.000000000000000000 ) ) ;
#390 = CYLINDRICAL_SURFACE ( 'NONE', #8511, 3.224098631618460331 ) ;
#391 = CARTESIAN_POINT ( 'NONE',  ( 0.000000000000000000, 0.000000000000000000, 283.5832628385307999 ) ) ;
#392 = ORIENTED_EDGE ( 'NONE', *, *, #15866, .T. ) ;
#393 = CARTESIAN_POINT ( 'NONE',  ( -141.8714406926361278, -48.70825716237272474, 39.99999999999999289 ) ) ;
#394 = VECTOR ( 'NONE', #11693, 1000.000000000000114 ) ;
#395 = ORIENTED_EDGE ( 'NONE', *, *, #3158, .T. ) ;
#396 = ORIENTED_EDGE ( 'NONE', *, *, #18390, .F. ) ;
#397 = CARTESIAN_POINT ( 'NONE',  ( 0.000000000000000000, 0.000000000000000000, 49.99999999999999289 ) ) ;
#398 = EDGE_CURVE ( 'NONE', #9612, #14697, #17220, .T. ) ;
#399 = VERTEX_POINT ( 'NONE', #1458 ) ;
#400 = ADVANCED_FACE ( 'NONE', ( #1248, #13721, #13823, #16903, #5862, #12074, #18338, #2794, #5963, #1667, #7484, #27, #3201, #9331, #6177, #16802, #18542, #15470, #12492, #4312, #4420, #19964, #12394, #18653, #4632, #18756, #12183, #7687, #7894, #10650, #10757, #18441, #7798, #9121, #15363, #1355, #7582 ), #17011, .F. ) ;
#401 = EDGE_CURVE ( 'NONE', #5555, #4348, #6279, .T. ) ;
#402 = LINE ( 'NONE', #6654, #2889 ) ;
#403 = DIRECTION ( 'NONE',  ( 1.000000000000000000, 0.000000000000000000, -0.000000000000000000 ) ) ;
#404 = ORIENTED_EDGE ( 'NONE', *, *, #17763, .T. ) ;
#405 =( NAMED_UNIT ( * ) PLANE_ANGLE_UNIT ( ) SI_UNIT ( $, .RADIAN. ) );
#406 = DIRECTION ( 'NONE',  ( -1.000000000000000000, 0.000000000000000000, 0.000000000000000000 ) ) ;
#407 = DIRECTION ( 'NONE',  ( 0.5300553768524375320, 0.8479630283625697595, 0.000000000000000000 ) ) ;
#409 = AXIS2_PLACEMENT_3D ( 'NONE', #4331, #19177, #450 ) ;
#408 = CARTESIAN_POINT ( 'NONE',  ( 49.07263256785952876, -39.37628763770437956, 248.9926560891072143 ) ) ;
#410 = VECTOR ( 'NONE', #17095, 1000.000000000000000 ) ;
#411 = DIRECTION ( 'NONE',  ( 0.000000000000000000, 0.000000000000000000, -1.000000000000000000 ) ) ;
#412 = DIRECTION ( 'NONE',  ( 0.3420201433256790380, -0.9396926207859046531, 0.000000000000000000 ) ) ;
#413 = ORIENTED_EDGE ( 'NONE', *, *, #34, .T. ) ;
#414 = DIRECTION ( 'NONE',  ( 1.000000000000000000, 0.000000000000000000, 0.000000000000000000 ) ) ;
#415 = ADVANCED_FACE ( 'NONE', ( #433 ), #17632, .T. ) ;
#416 = CARTESIAN_POINT ( 'NONE',  ( -11.73417718768092399, -61.81362617575098994, 132.4711112102474146 ) ) ;
#417 = VECTOR ( 'NONE', #16178, 1000.000000000000227 ) ;
#418 = CARTESIAN_POINT ( 'NONE',  ( -107.4999999999999716, -200.0000000000000000, 40.00000000000000000 ) ) ;
#419 = PLANE ( 'NONE',  #4671 ) ;
#420 = AXIS2_PLACEMENT_3D ( 'NONE', #20059, #15147, #19952 ) ;
#421 = ORIENTED_EDGE ( 'NONE', *, *, #14487, .F. ) ;
#422 = CARTESIAN_POINT ( 'NONE',  ( -110.0000000000000142, 285.0000000000000568, -82.50000000000001421 ) ) ;
#423 = CYLINDRICAL_SURFACE ( 'NONE', #14783, 77.50000000000000000 ) ;
#424 = ORIENTED_EDGE ( 'NONE', *, *, #11382, .F. ) ;
#425 = ORIENTED_EDGE ( 'NONE', *, *, #14850, .T. ) ;
#426 = ORIENTED_EDGE ( 'NONE', *, *, #9892, .F. ) ;
#427 = APPLICATION_PROTOCOL_DEFINITION ( 'draft international standard', 'automotive_design', 1998, #6727 ) ;
#428 = AXIS2_PLACEMENT_3D ( 'NONE', #8906, #8812, #13303 ) ;
#429 = AXIS2_PLACEMENT_3D ( 'NONE', #16436, #7119, #13337 ) ;
#430 = EDGE_CURVE ( 'NONE', #13898, #11413, #14350, .T. ) ;
#431 = ORIENTED_EDGE ( 'NONE', *, *, #9079, .T. ) ;
#432 = CARTESIAN_POINT ( 'NONE',  ( -68.18670162478832708, -38.41834839689356329, 248.9926560891072143 ) ) ;
#433 = FACE_OUTER_BOUND ( 'NONE', #9062, .T. ) ;
#434 = ORIENTED_EDGE ( 'NONE', *, *, #4227, .F. ) ;
#435 = DIRECTION ( 'NONE',  ( -1.000000000000000000, 0.000000000000000000, 0.000000000000000000 ) ) ;
#436 = FACE_OUTER_BOUND ( 'NONE', #18488, .T. ) ;
#437 = CARTESIAN_POINT ( 'NONE',  ( -98.17258311761709422, -133.0662226711790197, 6.375986368445647479 ) ) ;
#438 = EDGE_CURVE ( 'NONE', #5218, #9870, #5431, .T. ) ;
#439 = VECTOR ( 'NONE', #2770, 1000.000000000000114 ) ;
#440 = CARTESIAN_POINT ( 'NONE',  ( -122.1025966345561073, 68.49760859473882135, 37.84499468909948661 ) ) ;
#441 = FACE_OUTER_BOUND ( 'NONE', #8088, .T. ) ;
#442 = DIRECTION ( 'NONE',  ( -0.000000000000000000, -0.000000000000000000, -1.000000000000000000 ) ) ;
#443 = CARTESIAN_POINT ( 'NONE',  ( 52.50000000000000711, 6.293851260911244545E-13, -115.0000000000000000 ) ) ;
#444 = VECTOR ( 'NONE', #7066, 1000.000000000000000 ) ;
#445 = VECTOR ( 'NONE', #5247, 1000.000000000000000 ) ;
#446 = CARTESIAN_POINT ( 'NONE',  ( 19.63382932406841519, 18.38657833536341357, 39.88498244535531967 ) ) ;
#447 = DIRECTION ( 'NONE',  ( -1.000000000000000000, 0.000000000000000000, 0.000000000000000000 ) ) ;
#448 = FACE_OUTER_BOUND ( 'NONE', #5295, .T. ) ;
#449 = ORIENTED_EDGE ( 'NONE', *, *, #634, .T. ) ;
#450 = DIRECTION ( 'NONE',  ( 0.000000000000000000, 0.000000000000000000, -1.000000000000000000 ) ) ;
#451 = AXIS2_PLACEMENT_3D ( 'NONE', #4114, #2798, #845 ) ;
#452 = ORIENTED_EDGE ( 'NONE', *, *, #4347, .T. ) ;
#453 = APPLICATION_CONTEXT ( 'automotive_design' ) ;
#454 = ORIENTED_EDGE ( 'NONE', *, *, #3182, .F. ) ;
#455 = ORIENTED_EDGE ( 'NONE', *, *, #13971, .F. ) ;
#456 = DIRECTION ( 'NONE',  ( -0.7660444431189771253, 0.6427876096865404731, 5.349259755748777816E-15 ) ) ;
#457 = EDGE_CURVE ( 'NONE', #4545, #10038, #17552, .T. ) ;
#458 = CARTESIAN_POINT ( 'NONE',  ( -189.9999999999988916, 275.0000000000000000, 5.000000000000268230 ) ) ;
#459 = LINE ( 'NONE', #2301, #5504 ) ;
#460 = AXIS2_PLACEMENT_3D ( 'NONE', #12907, #17728, #3504 ) ;
#461 = CARTESIAN_POINT ( 'NONE',  ( -47.66508197439445382, 41.06890862491522398, 132.4711112102474146 ) ) ;
#462 = CARTESIAN_POINT ( 'NONE',  ( 22.81000261549368346, -58.63718168490493099, 132.4711112102474146 ) ) ;
#463 = DIRECTION ( 'NONE',  ( -0.000000000000000000, -0.000000000000000000, 1.000000000000000000 ) ) ;
#464 = CARTESIAN_POINT ( 'NONE',  ( 0.000000000000000000, 0.000000000000000000, -10.00000000000000178 ) ) ;
#465 = CIRCLE ( 'NONE', #17772, 3.224098631618455890 ) ;
#466 = FACE_OUTER_BOUND ( 'NONE', #14778, .T. ) ;
#467 = FACE_OUTER_BOUND ( 'NONE', #12951, .T. ) ;
#468 = ORIENTED_EDGE ( 'NONE', *, *, #8040, .F. ) ;
#469 = ADVANCED_FACE ( 'NONE', ( #4843 ), #3306, .F. ) ;
#470 = DIRECTION ( 'NONE',  ( 0.000000000000000000, 0.000000000000000000, 1.000000000000000000 ) ) ;
#471 = ORIENTED_EDGE ( 'NONE', *, *, #8214, .T. ) ;
#472 = EDGE_LOOP ( 'NONE', ( #15073, #6600, #4290, #1623 ) ) ;
#473 = VECTOR ( 'NONE', #13912, 1000.000000000000000 ) ;
#474 = ORIENTED_EDGE ( 'NONE', *, *, #16234, .F. ) ;
#475 = VECTOR ( 'NONE', #10571, 1000.000000000000114 ) ;
#476 = EDGE_LOOP ( 'NONE', ( #2456, #12768 ) ) ;
#477 = DIRECTION ( 'NONE',  ( 0.000000000000000000, 0.000000000000000000, -1.000000000000000000 ) ) ;
#478 = EDGE_CURVE ( 'NONE', #6273, #3496, #1532, .T. ) ;
#479 = LINE ( 'NONE', #10910, #17442 ) ;
#480 = EDGE_CURVE ( 'NONE', #10080, #12789, #2077, .T. ) ;
#481 = CARTESIAN_POINT ( 'NONE',  ( 39.84224160888901167, 67.36461649554546227, 110.9660488491356887 ) ) ;
#482 = DIRECTION ( 'NONE',  ( 1.000000000000000000, 0.000000000000000000, 0.000000000000000000 ) ) ;
#483 = ORIENTED_EDGE ( 'NONE', *, *, #16283, .F. ) ;
#484 = CARTESIAN_POINT ( 'NONE',  ( 134.7540465048387546, -65.88919983460813512, 5.016205221822248816 ) ) ;
#485 = CYLINDRICAL_SURFACE ( 'NONE', #1937, 3.224098631618460331 ) ;
#486 = ORIENTED_EDGE ( 'NONE', *, *, #8858, .T. ) ;
#487 = CARTESIAN_POINT ( 'NONE',  ( 0.000000000000000000, 0.000000000000000000, 293.5832628385307999 ) ) ;
#488 = CARTESIAN_POINT ( 'NONE',  ( 12.78021302872850562, -77.21438937758507848, 112.0427633081291816 ) ) ;
#489 = AXIS2_PLACEMENT_3D ( 'NONE', #7649, #18713, #18610 ) ;
#490 = DIRECTION ( 'NONE',  ( 0.000000000000000000, 0.000000000000000000, -1.000000000000000000 ) ) ;
#491 = DIRECTION ( 'NONE',  ( -1.000000000000000000, -0.000000000000000000, -0.000000000000000000 ) ) ;
#492 = EDGE_CURVE ( 'NONE', #11539, #4753, #17531, .T. ) ;
#493 = EDGE_CURVE ( 'NONE', #14511, #9172, #1973, .T. ) ;
#494 = CARTESIAN_POINT ( 'NONE',  ( -135.7837464099825695, -28.85345328491248651, -18.68477101865893175 ) ) ;
#495 = DIRECTION ( 'NONE',  ( -0.000000000000000000, -0.000000000000000000, 1.000000000000000000 ) ) ;
#496 = CARTESIAN_POINT ( 'NONE',  ( 93.27226090021298432, -117.4765369300808402, 48.33671567152951098 ) ) ;
#497 = ORIENTED_EDGE ( 'NONE', *, *, #17432, .F. ) ;
#498 = EDGE_CURVE ( 'NONE', #18312, #4139, #126, .T. ) ;
#499 = FACE_OUTER_BOUND ( 'NONE', #8497, .T. ) ;
#500 = ORIENTED_EDGE ( 'NONE', *, *, #7011, .T. ) ;
#501 = CIRCLE ( 'NONE', #1476, 17.50000000000000355 ) ;
#502 = ORIENTED_EDGE ( 'NONE', *, *, #7085, .F. ) ;
#503 = CARTESIAN_POINT ( 'NONE',  ( 0.000000000000000000, 0.000000000000000000, 132.4711112102474146 ) ) ;
#504 = AXIS2_PLACEMENT_3D ( 'NONE', #6795, #13106, #738 ) ;
#505 = EDGE_LOOP ( 'NONE', ( #8299, #8837, #2752, #9090 ) ) ;
#506 = EDGE_CURVE ( 'NONE', #2560, #13065, #10425, .T. ) ;
#507 = CARTESIAN_POINT ( 'NONE',  ( 1.379293853801755176, -78.26059000578311498, 112.7772637782949943 ) ) ;
#508 = EDGE_CURVE ( 'NONE', #5829, #10038, #8601, .T. ) ;
#509 = CARTESIAN_POINT ( 'NONE',  ( 0.000000000000000000, 0.000000000000000000, 283.5832628385307999 ) ) ;
#510 = DIRECTION ( 'NONE',  ( -0.000000000000000000, -0.000000000000000000, -1.000000000000000000 ) ) ;
#511 = DIRECTION ( 'NONE',  ( 0.000000000000000000, 1.000000000000000000, 0.000000000000000000 ) ) ;
#512 = DIRECTION ( 'NONE',  ( 0.000000000000000000, 0.000000000000000000, 1.000000000000000000 ) ) ;
#513 = PRODUCT ( 'Main Body', 'Main Body', '', ( #19350 ) ) ;
#514 = DIRECTION ( 'NONE',  ( 1.000000000000000000, 0.000000000000000000, 0.000000000000000000 ) ) ;
#515 = AXIS2_PLACEMENT_3D ( 'NONE', #5608, #10400, #8772 ) ;
#516 = DIRECTION ( 'NONE',  ( -0.000000000000000000, -0.000000000000000000, 1.000000000000000000 ) ) ;
#517 = CARTESIAN_POINT ( 'NONE',  ( 7.350000000000001421, 0.000000000000000000, 0.000000000000000000 ) ) ;
#518 = FACE_OUTER_BOUND ( 'NONE', #7990, .T. ) ;
#519 = CARTESIAN_POINT ( 'NONE',  ( 0.000000000000000000, 164.0736214083062805, 39.99999999999999289 ) ) ;
#520 = EDGE_CURVE ( 'NONE', #7250, #912, #6769, .T. ) ;
#521 = CARTESIAN_POINT ( 'NONE',  ( 0.000000000000000000, 0.000000000000000000, 283.5832628385307999 ) ) ;
#522 = LINE ( 'NONE', #8082, #10202 ) ;
#523 = ADVANCED_FACE ( 'NONE', ( #18020 ), #15040, .F. ) ;
#524 = ORIENTED_EDGE ( 'NONE', *, *, #19307, .F. ) ;
#525 = EDGE_CURVE ( 'NONE', #10391, #7427, #10330, .T. ) ;
#526 = DIRECTION ( 'NONE',  ( 0.000000000000000000, 1.000000000000000000, 0.000000000000000000 ) ) ;
#527 = CARTESIAN_POINT ( 'NONE',  ( -88.95069649744878859, 120.7914063265062055, 39.04816013673605113 ) ) ;
#528 = EDGE_LOOP ( 'NONE', ( #18695, #4336, #8989, #6164 ) ) ;
#529 = ORIENTED_EDGE ( 'NONE', *, *, #2169, .T. ) ;
#530 = EDGE_LOOP ( 'NONE', ( #18918, #10030, #2836 ) ) ;
#531 = PRODUCT_CONTEXT ( 'NONE', #16261, 'mechanical' ) ;
#532 = ORIENTED_EDGE ( 'NONE', *, *, #2284, .F. ) ;
#533 = AXIS2_PLACEMENT_3D ( 'NONE', #16138, #2125, #78 ) ;
#534 = LINE ( 'NONE', #13094, #8143 ) ;
#535 = EDGE_CURVE ( 'NONE', #93, #1238, #12637, .T. ) ;
#536 = CARTESIAN_POINT ( 'NONE',  ( -113.3498877299711864, 98.27513227905838278, 44.89206021334695862 ) ) ;
#537 = EDGE_LOOP ( 'NONE', ( #14888, #16258 ) ) ;
#538 = DIRECTION ( 'NONE',  ( 1.000000000000000000, 0.000000000000000000, -6.994638739193269649E-15 ) ) ;
#539 = DIRECTION ( 'NONE',  ( 0.9396926207859082059, 0.3420201433256694901, 0.000000000000000000 ) ) ;
#540 = CARTESIAN_POINT ( 'NONE',  ( -97.52847697650713599, -113.9950050385133693, 2.467650561764177741 ) ) ;
#541 = VERTEX_POINT ( 'NONE', #10137 ) ;
#542 = AXIS2_PLACEMENT_3D ( 'NONE', #2718, #18574, #10474 ) ;
#543 = DIRECTION ( 'NONE',  ( 0.1390141521205946196, -0.9902903945359624593, 0.000000000000000000 ) ) ;
#544 = DIRECTION ( 'NONE',  ( -0.6692498792541777819, -0.7430374143461878633, 0.000000000000000000 ) ) ;
#545 = AXIS2_PLACEMENT_3D ( 'NONE', #9683, #1507, #12750 ) ;
#546 = CARTESIAN_POINT ( 'NONE',  ( 159.9599531637113330, -36.50981547336952104, 39.99999999999999289 ) ) ;
#547 = EDGE_CURVE ( 'NONE', #14566, #10313, #13391, .T. ) ;
#548 = EDGE_CURVE ( 'NONE', #12640, #16017, #8706, .T. ) ;
#549 = CARTESIAN_POINT ( 'NONE',  ( 47.56406379474552182, 37.78325588002191893, 293.5832628385307999 ) ) ;
#550 = CARTESIAN_POINT ( 'NONE',  ( 0.000000000000000000, 0.000000000000000000, 293.5832628385307999 ) ) ;
#551 = FACE_OUTER_BOUND ( 'NONE', #9374, .T. ) ;
#552 = EDGE_LOOP ( 'NONE', ( #7577, #5145, #8695, #8498 ) ) ;
#553 = AXIS2_PLACEMENT_3D ( 'NONE', #18898, #14285, #12937 ) ;
#554 = CARTESIAN_POINT ( 'NONE',  ( -41.06890862491505345, -47.66508197439457462, 248.9926560891072143 ) ) ;
#555 = EDGE_CURVE ( 'NONE', #13410, #10176, #5141, .T. ) ;
#556 = ORIENTED_EDGE ( 'NONE', *, *, #14355, .F. ) ;
#557 = VECTOR ( 'NONE', #16246, 1000.000000000000000 ) ;
#558 = EDGE_LOOP ( 'NONE', ( #486, #1812, #16928, #3761 ) ) ;
#559 = AXIS2_PLACEMENT_3D ( 'NONE', #821, #3898, #19644 ) ;
#560 = ORIENTED_EDGE ( 'NONE', *, *, #15092, .F. ) ;
#561 = AXIS2_PLACEMENT_3D ( 'NONE', #312, #4936, #6361 ) ;
#562 = CARTESIAN_POINT ( 'NONE',  ( -32.30548103355237544, 113.3261241031799926, 14.88498244535567672 ) ) ;
#563 = CARTESIAN_POINT ( 'NONE',  ( 59.51724408343574879, -12.14957802882732452, 283.5832628385307999 ) ) ;
#564 = DIRECTION ( 'NONE',  ( -0.000000000000000000, -1.000000000000000000, -0.000000000000000000 ) ) ;
#565 = DIRECTION ( 'NONE',  ( -0.000000000000000000, -1.000000000000000000, -0.000000000000000000 ) ) ;
#566 = CARTESIAN_POINT ( 'NONE',  ( 140.0000000000000284, 0.000000000000000000, -115.0000000000000142 ) ) ;
#567 = PLANE ( 'NONE',  #6525 ) ;
#568 = LINE ( 'NONE', #2209, #10145 ) ;
#569 = LINE ( 'NONE', #8032, #16267 ) ;
#570 = ORIENTED_EDGE ( 'NONE', *, *, #11345, .F. ) ;
#571 = ORIENTED_EDGE ( 'NONE', *, *, #2295, .T. ) ;
#572 = AXIS2_PLACEMENT_3D ( 'NONE', #19392, #3830, #12091 ) ;
#573 = VERTEX_POINT ( 'NONE', #17823 ) ;
#574 = ORIENTED_EDGE ( 'NONE', *, *, #37, .T. ) ;
#575 = ORIENTED_EDGE ( 'NONE', *, *, #4277, .F. ) ;
#576 = DIRECTION ( 'NONE',  ( -0.6427876096865328126, -0.7660444431189835646, 0.000000000000000000 ) ) ;
#577 = DIRECTION ( 'NONE',  ( -0.5000000000000101030, 0.8660254037844328234, 0.000000000000000000 ) ) ;
#578 = DIRECTION ( 'NONE',  ( 0.9749279121818257288, -0.2225209339563047339, 0.000000000000000000 ) ) ;
#579 = ORIENTED_EDGE ( 'NONE', *, *, #19467, .F. ) ;
#580 = LINE ( 'NONE', #2325, #4763 ) ;
#581 = LINE ( 'NONE', #8155, #8466 ) ;
#582 = AXIS2_PLACEMENT_3D ( 'NONE', #17065, #9285, #15422 ) ;
#583 = ORIENTED_EDGE ( 'NONE', *, *, #19634, .T. ) ;
#584 = CARTESIAN_POINT ( 'NONE',  ( -93.38451287766530129, 109.3625709609712544, -31.42891559531335588 ) ) ;
#585 = LINE ( 'NONE', #17782, #14674 ) ;
#586 = DIRECTION ( 'NONE',  ( 1.000000000000000000, 0.000000000000000000, 0.000000000000000000 ) ) ;
#587 = LINE ( 'NONE', #10456, #10288 ) ;
#588 = CARTESIAN_POINT ( 'NONE',  ( -136.9468171063203101, -26.51361207507547491, -17.34057338814886862 ) ) ;
#589 = LINE ( 'NONE', #11628, #17406 ) ;
#590 = CARTESIAN_POINT ( 'NONE',  ( 99.70727046260189752, -112.0668231182905572, 49.97544513886636963 ) ) ;
#591 = ORIENTED_EDGE ( 'NONE', *, *, #10844, .T. ) ;
#592 = EDGE_CURVE ( 'NONE', #9122, #5287, #632, .T. ) ;
#593 = CARTESIAN_POINT ( 'NONE',  ( 0.07568653364412687712, -1.751902528157470718, -8.999999999999998224 ) ) ;
#594 = ORIENTED_EDGE ( 'NONE', *, *, #16874, .F. ) ;
#595 = AXIS2_PLACEMENT_3D ( 'NONE', #1167, #16828, #19689 ) ;
#596 = ORIENTED_EDGE ( 'NONE', *, *, #14234, .T. ) ;
#597 = LINE ( 'NONE', #3867, #11838 ) ;
#598 = VECTOR ( 'NONE', #5827, 1000.000000000000000 ) ;
#599 = VERTEX_POINT ( 'NONE', #13287 ) ;
#600 = FACE_OUTER_BOUND ( 'NONE', #14957, .T. ) ;
#601 = EDGE_CURVE ( 'NONE', #16327, #219, #6106, .T. ) ;
#602 = CARTESIAN_POINT ( 'NONE',  ( -82.33470881469955316, -125.3834122142802272, 33.60191280747055487 ) ) ;
#603 = ADVANCED_FACE ( 'NONE', ( #10043 ), #11851, .T. ) ;
#604 = CARTESIAN_POINT ( 'NONE',  ( 0.000000000000000000, 0.000000000000000000, 132.4711112102474146 ) ) ;
#605 = EDGE_CURVE ( 'NONE', #13307, #14163, #11759, .T. ) ;
#606 = CARTESIAN_POINT ( 'NONE',  ( -45.46712722958807973, 40.27908801170008957, 283.5832628385307999 ) ) ;
#607 = DIRECTION ( 'NONE',  ( -0.3420201433256601642, -0.9396926207859114255, 0.000000000000000000 ) ) ;
#608 = CARTESIAN_POINT ( 'NONE',  ( 104.1558342746901928, -124.2522228486704421, 0.5619391425930568840 ) ) ;
#609 = CIRCLE ( 'NONE', #7461, 34.99999999999997868 ) ;
#610 = AXIS2_PLACEMENT_3D ( 'NONE', #18415, #15333, #2864 ) ;
#611 = VECTOR ( 'NONE', #4918, 1000.000000000000000 ) ;
#612 = LINE ( 'NONE', #19529, #7209 ) ;
#613 = DIRECTION ( 'NONE',  ( -6.982962677686266711E-15, 0.000000000000000000, -1.000000000000000000 ) ) ;
#614 = AXIS2_PLACEMENT_3D ( 'NONE', #2103, #14577, #4975 ) ;
#615 = FACE_OUTER_BOUND ( 'NONE', #9474, .T. ) ;
#616 = DIRECTION ( 'NONE',  ( 0.000000000000000000, 0.000000000000000000, 1.000000000000000000 ) ) ;
#617 = DIRECTION ( 'NONE',  ( 1.000000000000000000, 0.000000000000000000, 0.000000000000000000 ) ) ;
#618 = CARTESIAN_POINT ( 'NONE',  ( 93.45568245711652366, -117.3306176392091373, 48.42050290853573102 ) ) ;
#619 = ORIENTED_EDGE ( 'NONE', *, *, #10225, .F. ) ;
#620 = ADVANCED_FACE ( 'NONE', ( #10231 ), #2366, .T. ) ;
#621 = LINE ( 'NONE', #8495, #13010 ) ;
#622 = FACE_OUTER_BOUND ( 'NONE', #12847, .T. ) ;
#623 = ORIENTED_EDGE ( 'NONE', *, *, #12748, .F. ) ;
#624 = EDGE_LOOP ( 'NONE', ( #7544, #7506, #16288, #12643 ) ) ;
#625 = VERTEX_POINT ( 'NONE', #8798 ) ;
#626 = ITEM_DEFINED_TRANSFORMATION ( 'NONE', 'NONE', #4628,  #18639 ) ;
#627 = VECTOR ( 'NONE', #3562, 1000.000000000000000 ) ;
#628 = AXIS2_PLACEMENT_3D ( 'NONE', #13240, #7026, #19693 ) ;
#629 = DIRECTION ( 'NONE',  ( -0.9511061040868804550, -0.3088643371590125697, 0.000000000000000000 ) ) ;
#630 = VECTOR ( 'NONE', #14767, 1000.000000000000114 ) ;
#631 = EDGE_CURVE ( 'NONE', #14818, #6254, #14743, .T. ) ;
#632 = LINE ( 'NONE', #19353, #1191 ) ;
#633 = EDGE_LOOP ( 'NONE', ( #11208, #14397, #3955, #8739 ) ) ;
#634 = EDGE_CURVE ( 'NONE', #17381, #14953, #13488, .T. ) ;
#635 = LINE ( 'NONE', #17826, #1419 ) ;
#636 = CARTESIAN_POINT ( 'NONE',  ( 60.68773558783009747, -2.629322876227576433, 283.5832628385307999 ) ) ;
#637 = CARTESIAN_POINT ( 'NONE',  ( -95.49560220037844260, -115.9193184531315381, 6.561900623234592445 ) ) ;
#638 = ORIENTED_EDGE ( 'NONE', *, *, #4760, .F. ) ;
#639 = EDGE_CURVE ( 'NONE', #4730, #9351, #19739, .T. ) ;
#640 = LINE ( 'NONE', #13102, #7507 ) ;
#641 = CARTESIAN_POINT ( 'NONE',  ( -113.3514208120937781, -17.29894464209964866, 14.88498244535624337 ) ) ;
#642 = CARTESIAN_POINT ( 'NONE',  ( -110.0000000000000142, 275.0000000000000000, 5.000000000000000888 ) ) ;
#643 =( NAMED_UNIT ( * ) SI_UNIT ( $, .STERADIAN. ) SOLID_ANGLE_UNIT ( ) );
#644 = CARTESIAN_POINT ( 'NONE',  ( -0.8220851292435327196, -78.26059000578311498, 248.9926560891072143 ) ) ;
#645 = AXIS2_PLACEMENT_3D ( 'NONE', #919, #2868, #2668 ) ;
#646 = LINE ( 'NONE', #6889, #1478 ) ;
#647 = VECTOR ( 'NONE', #10889, 1000.000000000000114 ) ;
#648 = VERTEX_POINT ( 'NONE', #17925 ) ;
#649 = EDGE_CURVE ( 'NONE', #11180, #14061, #3174, .T. ) ;
#650 = DIRECTION ( 'NONE',  ( -6.982962677686266711E-15, 0.000000000000000000, -1.000000000000000000 ) ) ;
#651 = ORIENTED_EDGE ( 'NONE', *, *, #11384, .F. ) ;
#652 = ORIENTED_EDGE ( 'NONE', *, *, #1769, .F. ) ;
#653 = ORIENTED_EDGE ( 'NONE', *, *, #1354, .F. ) ;
#654 = ADVANCED_FACE ( 'NONE', ( #7666 ), #12466, .F. ) ;
#655 = DIRECTION ( 'NONE',  ( -0.000000000000000000, -1.000000000000000000, -0.000000000000000000 ) ) ;
#656 = EDGE_CURVE ( 'NONE', #12589, #3734, #6149, .T. ) ;
#657 = CARTESIAN_POINT ( 'NONE',  ( -126.0064496073183591, -81.39031533630314641, -9.417289231373237257 ) ) ;
#658 = CARTESIAN_POINT ( 'NONE',  ( -20.84572577951200500, -54.86954475316249358, 132.4711112102474146 ) ) ;
#659 = CARTESIAN_POINT ( 'NONE',  ( -136.4994460260996902, -31.11111111111110006, -10.83394172763413899 ) ) ;
#660 = EDGE_CURVE ( 'NONE', #17410, #15549, #8916, .T. ) ;
#661 = ORIENTED_EDGE ( 'NONE', *, *, #1097, .F. ) ;
#662 = DIRECTION ( 'NONE',  ( -0.000000000000000000, -0.000000000000000000, 1.000000000000000000 ) ) ;
#663 = CARTESIAN_POINT ( 'NONE',  ( -129.0037046021669767, -76.61892870327682203, -0.1306340574592130821 ) ) ;
#664 = CARTESIAN_POINT ( 'NONE',  ( 134.6385828715892217, -73.56429320930371318, 7.599106732516738738 ) ) ;
#665 = PLANE ( 'NONE',  #18608 ) ;
#666 = CARTESIAN_POINT ( 'NONE',  ( -176.7850001792984358, -194.3449193228699414, 2.490758961397592675 ) ) ;
#667 = PLANE ( 'NONE',  #2202 ) ;
#668 = PRODUCT_DEFINITION_CONTEXT ( 'detailed design', #4634, 'design' ) ;
#669 = ORIENTED_EDGE ( 'NONE', *, *, #5124, .F. ) ;
#670 = VECTOR ( 'NONE', #2856, 1000.000000000000114 ) ;
#671 = PRODUCT_DEFINITION_FORMATION_WITH_SPECIFIED_SOURCE ( 'ANY', '', #15700, .NOT_KNOWN. ) ;
#672 = VECTOR ( 'NONE', #9418, 1000.000000000000000 ) ;
#673 = ORIENTED_EDGE ( 'NONE', *, *, #8391, .F. ) ;
#674 = ORIENTED_EDGE ( 'NONE', *, *, #4626, .F. ) ;
#675 = VERTEX_POINT ( 'NONE', #13593 ) ;
#676 = ORIENTED_EDGE ( 'NONE', *, *, #9749, .T. ) ;
#677 = DIRECTION ( 'NONE',  ( -0.9848077530122097967, 0.1736481776669207000, 0.000000000000000000 ) ) ;
#678 = AXIS2_PLACEMENT_3D ( 'NONE', #19949, #2979, #9000 ) ;
#679 = LINE ( 'NONE', #6924, #9296 ) ;
#680 = DIRECTION ( 'NONE',  ( -1.000000000000000000, 0.000000000000000000, 0.000000000000000000 ) ) ;
#681 = ORIENTED_EDGE ( 'NONE', *, *, #13967, .F. ) ;
#682 = AXIS2_PLACEMENT_3D ( 'NONE', #5183, #17564, #3537 ) ;
#683 = LINE ( 'NONE', #6927, #6077 ) ;
#684 = CARTESIAN_POINT ( 'NONE',  ( 39.84224160888901167, 67.36461649554546227, 132.4711112102474146 ) ) ;
#685 = EDGE_CURVE ( 'NONE', #3831, #739, #15136, .T. ) ;
#686 = EDGE_LOOP ( 'NONE', ( #4759, #20168, #5378, #19082, #13161, #7782, #5172, #267, #1533, #7449, #5941, #583, #3735, #5761, #17193, #6714, #16858, #15007, #1728, #12781, #8037, #18671, #16578, #19251, #1715, #18339, #12228, #4895, #11794, #7815, #748, #14906, #395 ) ) ;
#687 = DIRECTION ( 'NONE',  ( -0.3420201433256757073, 0.9396926207859057634, 0.000000000000000000 ) ) ;
#688 = LINE ( 'NONE', #5693, #18512 ) ;
#689 = DIRECTION ( 'NONE',  ( -0.000000000000000000, -0.000000000000000000, 1.000000000000000000 ) ) ;
#690 = DIRECTION ( 'NONE',  ( -0.000000000000000000, -0.000000000000000000, 1.000000000000000000 ) ) ;
#691 = CARTESIAN_POINT ( 'NONE',  ( -34.51244174799990816, 110.9757759606085017, 14.88498244535569093 ) ) ;
#692 = DIRECTION ( 'NONE',  ( -0.7660444431189766812, 0.6427876096865408062, 4.304393070272782536E-15 ) ) ;
#693 = DIRECTION ( 'NONE',  ( -0.03505990758545545621, -0.9993852124581888985, 0.000000000000000000 ) ) ;
#694 = ORIENTED_EDGE ( 'NONE', *, *, #7836, .T. ) ;
#695 = VECTOR ( 'NONE', #18044, 1000.000000000000114 ) ;
#696 = DIRECTION ( 'NONE',  ( 0.7818314824680220321, 0.6234898018587433643, 0.000000000000000000 ) ) ;
#697 = ORIENTED_EDGE ( 'NONE', *, *, #18645, .T. ) ;
#698 = VERTEX_POINT ( 'NONE', #1222 ) ;
#699 = FACE_OUTER_BOUND ( 'NONE', #9006, .T. ) ;
#700 = ORIENTED_EDGE ( 'NONE', *, *, #19231, .F. ) ;
#701 = LINE ( 'NONE', #8276, #10766 ) ;
#702 = CARTESIAN_POINT ( 'NONE',  ( 7.950000000000000178, 0.000000000000000000, 0.000000000000000000 ) ) ;
#703 = PLANE ( 'NONE',  #4090 ) ;
#704 = LINE ( 'NONE', #17603, #2792 ) ;
#705 = EDGE_CURVE ( 'NONE', #182, #6905, #10519, .T. ) ;
#706 = ORIENTED_EDGE ( 'NONE', *, *, #12017, .T. ) ;
#707 = LINE ( 'NONE', #5926, #14264 ) ;
#708 = CARTESIAN_POINT ( 'NONE',  ( 103.6579813550140017, -125.0534741538843235, 0.7510394427105699933 ) ) ;
#709 = DIRECTION ( 'NONE',  ( 0.1736481776669273336, 0.9848077530122085754, 0.000000000000000000 ) ) ;
#710 = CARTESIAN_POINT ( 'NONE',  ( 54.86954475316255042, -20.84572577951183092, 111.4180192758974499 ) ) ;
#711 = ORIENTED_EDGE ( 'NONE', *, *, #14248, .F. ) ;
#712 = CARTESIAN_POINT ( 'NONE',  ( 51.24245927909996112, -32.62092819947974220, 293.5832628385307999 ) ) ;
#713 = CARTESIAN_POINT ( 'NONE',  ( 97.50000000000001421, -133.9542832461881119, 30.00000000000000000 ) ) ;
#714 = CARTESIAN_POINT ( 'NONE',  ( 82.22461745850688430, -125.4556360547411344, 7.112305957179646754 ) ) ;
#715 = CARTESIAN_POINT ( 'NONE',  ( 3.123743752084377601, -4.811834253409482010, 293.5832628385307999 ) ) ;
#716 = ORIENTED_EDGE ( 'NONE', *, *, #9383, .F. ) ;
#717 = ADVANCED_FACE ( 'NONE', ( #15338 ), #19942, .F. ) ;
#718 = DIRECTION ( 'NONE',  ( -0.9749279121818223981, -0.2225209339563194721, 0.000000000000000000 ) ) ;
#719 = LINE ( 'NONE', #8496, #5976 ) ;
#720 = VERTEX_POINT ( 'NONE', #7362 ) ;
#721 = ORIENTED_EDGE ( 'NONE', *, *, #8886, .T. ) ;
#722 = CARTESIAN_POINT ( 'NONE',  ( 101.0196388379316659, 100.9199429146863167, 49.99999999999999289 ) ) ;
#723 = DIRECTION ( 'NONE',  ( 0.7660444431189707970, 0.6427876096865481337, 0.000000000000000000 ) ) ;
#724 = CIRCLE ( 'NONE', #19044, 3.224098631618458999 ) ;
#725 = ORIENTED_EDGE ( 'NONE', *, *, #984, .T. ) ;
#726 = VECTOR ( 'NONE', #11409, 999.9999999999998863 ) ;
#727 = CARTESIAN_POINT ( 'NONE',  ( 96.59911734864401467, -114.8254675080909095, 3.766286132638113848 ) ) ;
#728 = CARTESIAN_POINT ( 'NONE',  ( 58.63718168490485283, 22.81000261549389307, 248.9926560891072143 ) ) ;
#729 = CARTESIAN_POINT ( 'NONE',  ( -95.77047472624724378, -116.1200526047209394, 9.227179618507987513 ) ) ;
#730 = ORIENTED_EDGE ( 'NONE', *, *, #1243, .F. ) ;
#731 = EDGE_CURVE ( 'NONE', #19514, #5793, #7459, .T. ) ;
#732 = AXIS2_PLACEMENT_3D ( 'NONE', #11861, #13300, #19653 ) ;
#733 = DIRECTION ( 'NONE',  ( -0.000000000000000000, -0.000000000000000000, -1.000000000000000000 ) ) ;
#734 = DIRECTION ( 'NONE',  ( -6.982962677686265922E-15, -1.972152263052529514E-31, -1.000000000000000000 ) ) ;
#735 = CARTESIAN_POINT ( 'NONE',  ( 23.23469325536214214, -13.41455640552199924, 14.88498244535528947 ) ) ;
#736 = CARTESIAN_POINT ( 'NONE',  ( -31.86742755225479584, 24.93940645478156526, 248.9926560891072143 ) ) ;
#737 = CARTESIAN_POINT ( 'NONE',  ( -15.91767397667354800, 141.9028892025177413, 49.99999999999999289 ) ) ;
#738 = DIRECTION ( 'NONE',  ( 0.5000000000000038858, 0.8660254037844363761, -3.520662956770155909E-15 ) ) ;
#739 = VERTEX_POINT ( 'NONE', #18318 ) ;
#740 = EDGE_CURVE ( 'NONE', #961, #7600, #11543, .T. ) ;
#741 = CARTESIAN_POINT ( 'NONE',  ( 141.8714406926368099, -48.70825716237082759, 60.00000000000000000 ) ) ;
#742 = CARTESIAN_POINT ( 'NONE',  ( 7.350000000000000533, 5.196152422706624030, -9.000000000000001776 ) ) ;
#743 = CIRCLE ( 'NONE', #20010, 15.91767397667354089 ) ;
#744 = VECTOR ( 'NONE', #7674, 1000.000000000000114 ) ;
#745 = EDGE_CURVE ( 'NONE', #1745, #14667, #18421, .T. ) ;
#746 = AXIS2_PLACEMENT_3D ( 'NONE', #2840, #16555, #12127 ) ;
#747 = ORIENTED_EDGE ( 'NONE', *, *, #8839, .T. ) ;
#748 = ORIENTED_EDGE ( 'NONE', *, *, #13971, .T. ) ;
#749 = CARTESIAN_POINT ( 'NONE',  ( 92.34802049131684498, -66.64338626758360817, 14.88498244535480630 ) ) ;
#750 = EDGE_CURVE ( 'NONE', #5911, #17872, #1330, .T. ) ;
#751 = CARTESIAN_POINT ( 'NONE',  ( -126.7590367374602494, -80.21250349114244216, -9.076491356015703005 ) ) ;
#752 = DIRECTION ( 'NONE',  ( 0.000000000000000000, 0.000000000000000000, 1.000000000000000000 ) ) ;
#753 = CIRCLE ( 'NONE', #11206, 7.500000000000006217 ) ;
#754 = DIRECTION ( 'NONE',  ( 6.982962677686266711E-15, -0.000000000000000000, 1.000000000000000000 ) ) ;
#755 = DIRECTION ( 'NONE',  ( 0.3427509529624095941, 0.9394263059140722794, 0.000000000000000000 ) ) ;
#756 = DIRECTION ( 'NONE',  ( 0.9396926207859114255, -0.3420201433256601642, 0.000000000000000000 ) ) ;
#757 = CARTESIAN_POINT ( 'NONE',  ( -77.50000000000000000, 9.491012693391988181E-15, -100.0000000000000000 ) ) ;
#758 = VECTOR ( 'NONE', #990, 1000.000000000000000 ) ;
#759 = CARTESIAN_POINT ( 'NONE',  ( -26.42151830275515323, 4.658826548058537576, 14.88498244535563586 ) ) ;
#760 = CARTESIAN_POINT ( 'NONE',  ( 56.84754764479241373, -154.7316448359447634, 60.00000000000000000 ) ) ;
#761 = EDGE_LOOP ( 'NONE', ( #20006, #19054, #13041 ) ) ;
#762 = EDGE_CURVE ( 'NONE', #18014, #5623, #16769, .T. ) ;
#763 = EDGE_CURVE ( 'NONE', #9877, #8052, #9249, .T. ) ;
#764 = EDGE_CURVE ( 'NONE', #14186, #1114, #6047, .T. ) ;
#765 = ORIENTED_EDGE ( 'NONE', *, *, #6498, .T. ) ;
#766 = CIRCLE ( 'NONE', #13818, 7.500000000000000000 ) ;
#767 = ORIENTED_EDGE ( 'NONE', *, *, #1905, .T. ) ;
#768 = ORIENTED_EDGE ( 'NONE', *, *, #10405, .F. ) ;
#769 = CARTESIAN_POINT ( 'NONE',  ( 14.39940464655707331, 76.92888220842492331, 112.0427633081292953 ) ) ;
#770 = EDGE_LOOP ( 'NONE', ( #15637, #2166, #12568, #2461 ) ) ;
#771 = AXIS2_PLACEMENT_3D ( 'NONE', #14466, #6901, #11492 ) ;
#772 = EDGE_CURVE ( 'NONE', #1021, #8910, #10828, .T. ) ;
#773 = LINE ( 'NONE', #10087, #5009 ) ;
#774 = CARTESIAN_POINT ( 'NONE',  ( -36.99387960884161686, 48.17797692984174773, 283.5832628385307999 ) ) ;
#775 = AXIS2_PLACEMENT_3D ( 'NONE', #10807, #9387, #14194 ) ;
#776 = DIRECTION ( 'NONE',  ( -0.000000000000000000, -0.000000000000000000, -1.000000000000000000 ) ) ;
#777 = ORIENTED_EDGE ( 'NONE', *, *, #9922, .T. ) ;
#778 = DIRECTION ( 'NONE',  ( 1.000000000000000000, 0.000000000000000000, 0.000000000000000000 ) ) ;
#779 = PLANE ( 'NONE',  #17644 ) ;
#780 = ORIENTED_EDGE ( 'NONE', *, *, #16980, .F. ) ;
#781 = PLANE ( 'NONE',  #11393 ) ;
#782 = PLANE ( 'NONE',  #19179 ) ;
#783 = DIRECTION ( 'NONE',  ( 1.000000000000000000, 0.000000000000000000, 0.000000000000000000 ) ) ;
#784 = AXIS2_PLACEMENT_3D ( 'NONE', #1960, #6363, #6465 ) ;
#785 = LINE ( 'NONE', #7034, #12769 ) ;
#786 = EDGE_CURVE ( 'NONE', #18064, #15547, #13824, .T. ) ;
#787 = CARTESIAN_POINT ( 'NONE',  ( 2.240720816136066773, -5.281164089014820817, 293.5832628385307999 ) ) ;
#788 = DIRECTION ( 'NONE',  ( -0.8660254037844328234, -0.5000000000000101030, 0.000000000000000000 ) ) ;
#789 = ORIENTED_EDGE ( 'NONE', *, *, #13137, .T. ) ;
#790 = CARTESIAN_POINT ( 'NONE',  ( -63.98537287693023501, 94.20918150411493741, 39.88498244535590231 ) ) ;
#791 = VECTOR ( 'NONE', #6303, 1000.000000000000000 ) ;
#792 = ORIENTED_EDGE ( 'NONE', *, *, #6721, .T. ) ;
#793 = ADVANCED_FACE ( 'NONE', ( #9201 ), #15445, .T. ) ;
#794 = ORIENTED_EDGE ( 'NONE', *, *, #4681, .F. ) ;
#795 = DIRECTION ( 'NONE',  ( -0.000000000000000000, -0.000000000000000000, 1.000000000000000000 ) ) ;
#796 = VERTEX_POINT ( 'NONE', #3075 ) ;
#797 = CARTESIAN_POINT ( 'NONE',  ( -9.176097008933940202, -25.21111933077039069, 39.88498244535551862 ) ) ;
#798 = CARTESIAN_POINT ( 'NONE',  ( 128.2779226595531270, 102.2982297021113141, 60.00000000000000000 ) ) ;
#799 = AXIS2_PLACEMENT_3D ( 'NONE', #5132, #17310, #9715 ) ;
#800 = FACE_OUTER_BOUND ( 'NONE', #13112, .T. ) ;
#801 = DIRECTION ( 'NONE',  ( -0.000000000000000000, -1.000000000000000000, -0.000000000000000000 ) ) ;
#802 = ORIENTED_EDGE ( 'NONE', *, *, #15206, .F. ) ;
#803 = CARTESIAN_POINT ( 'NONE',  ( -130.1901167961280521, -74.50443780700842922, 46.26218360866808865 ) ) ;
#804 = CARTESIAN_POINT ( 'NONE',  ( 63.68887634719570912, -147.8252249328912740, 39.99999999999999289 ) ) ;
#805 = CARTESIAN_POINT ( 'NONE',  ( 60.72279549541555355, -1.629937663769388090, 293.5832628385307999 ) ) ;
#806 = LINE ( 'NONE', #906, #1790 ) ;
#807 = VERTEX_POINT ( 'NONE', #18628 ) ;
#808 = CARTESIAN_POINT ( 'NONE',  ( -144.1130761623740568, -69.50842595698578918, 49.99999999999999289 ) ) ;
#809 = CARTESIAN_POINT ( 'NONE',  ( 56.12853591711344592, -23.22718332831461652, 283.5832628385307999 ) ) ;
#810 = CARTESIAN_POINT ( 'NONE',  ( 82.03125000000005684, -125.5821405433014064, 9.272053618398000907 ) ) ;
#811 = CIRCLE ( 'NONE', #18457, 99.99999999999997158 ) ;
#812 = PLANE ( 'NONE',  #20001 ) ;
#813 = ORIENTED_EDGE ( 'NONE', *, *, #1509, .F. ) ;
#814 = PLANE ( 'NONE',  #7143 ) ;
#815 = CARTESIAN_POINT ( 'NONE',  ( -29.99999999999887379, 275.0000000000000000, 4.999999999999158007 ) ) ;
#816 = ORIENTED_EDGE ( 'NONE', *, *, #10481, .T. ) ;
#817 = VECTOR ( 'NONE', #13786, 999.9999999999998863 ) ;
#818 = VERTEX_POINT ( 'NONE', #9309 ) ;
#819 = ORIENTED_EDGE ( 'NONE', *, *, #12411, .T. ) ;
#820 = DIRECTION ( 'NONE',  ( 1.000000000000000000, 0.000000000000000000, -0.000000000000000000 ) ) ;
#821 = CARTESIAN_POINT ( 'NONE',  ( 0.000000000000000000, 0.000000000000000000, 283.5832628385307999 ) ) ;
#822 = ORIENTED_EDGE ( 'NONE', *, *, #13054, .T. ) ;
#823 = VECTOR ( 'NONE', #11548, 1000.000000000000000 ) ;
#824 = CARTESIAN_POINT ( 'NONE',  ( 95.45795901651801785, -116.1130648478386007, 7.867509371635869719 ) ) ;
#825 = CARTESIAN_POINT ( 'NONE',  ( -100.4426743477017965, -129.9257371803582259, 2.884579890773657507 ) ) ;
#826 =( REPRESENTATION_RELATIONSHIP ('NONE','NONE', #17382, #2084 ) REPRESENTATION_RELATIONSHIP_WITH_TRANSFORMATION ( #19062 )SHAPE_REPRESENTATION_RELATIONSHIP( ) );
#827 = CARTESIAN_POINT ( 'NONE',  ( -150.0000000000000284, 0.000000000000000000, 49.99999999999999289 ) ) ;
#828 = CARTESIAN_POINT ( 'NONE',  ( 0.000000000000000000, 0.000000000000000000, 283.5832628385307999 ) ) ;
#829 = CARTESIAN_POINT ( 'NONE',  ( 51.51682027493064453, -28.15057869795607459, 110.9660488491357455 ) ) ;
#830 = DIRECTION ( 'NONE',  ( 0.000000000000000000, 0.000000000000000000, -1.000000000000000000 ) ) ;
#831 = FACE_OUTER_BOUND ( 'NONE', #15190, .T. ) ;
#832 = DIRECTION ( 'NONE',  ( -0.000000000000000000, -0.000000000000000000, 1.000000000000000000 ) ) ;
#833 = AXIS2_PLACEMENT_3D ( 'NONE', #13835, #20185, #6186 ) ;
#834 = EDGE_LOOP ( 'NONE', ( #11102, #16029, #13341, #7575, #11239, #15936 ) ) ;
#835 = CARTESIAN_POINT ( 'NONE',  ( -28.94886449118902760, 53.40063514825087765, 293.5832628385307999 ) ) ;
#836 = DIRECTION ( 'NONE',  ( -0.000000000000000000, -0.000000000000000000, 1.000000000000000000 ) ) ;
#837 =( GEOMETRIC_REPRESENTATION_CONTEXT ( 3 ) GLOBAL_UNCERTAINTY_ASSIGNED_CONTEXT ( ( #2726 ) ) GLOBAL_UNIT_ASSIGNED_CONTEXT ( ( #7973, #15755, #14217 ) ) REPRESENTATION_CONTEXT ( 'NONE', 'WORKASPACE' ) );
#838 = EDGE_CURVE ( 'NONE', #12583, #959, #9515, .T. ) ;
#839 = ORIENTED_EDGE ( 'NONE', *, *, #18273, .F. ) ;
#840 = ORIENTED_EDGE ( 'NONE', *, *, #17283, .T. ) ;
#841 = ADVANCED_FACE ( 'NONE', ( #8070 ), #14323, .T. ) ;
#842 = LINE ( 'NONE', #11976, #13920 ) ;
#843 = ORIENTED_EDGE ( 'NONE', *, *, #14946, .T. ) ;
#844 = EDGE_CURVE ( 'NONE', #15222, #12174, #8270, .T. ) ;
#845 = DIRECTION ( 'NONE',  ( 1.000000000000000000, 0.000000000000000000, -6.994638739193269649E-15 ) ) ;
#846 = LINE ( 'NONE', #3630, #15499 ) ;
#847 = ADVANCED_FACE ( 'NONE', ( #7869, #100, #5022, #11349, #3578, #17601, #304, #15753 ), #19234, .F. ) ;
#848 = LINE ( 'NONE', #17748, #13020 ) ;
#849 = ADVANCED_FACE ( 'NONE', ( #11448 ), #1947, .T. ) ;
#850 = CARTESIAN_POINT ( 'NONE',  ( -63.98537287693023501, 94.20918150411493741, 39.88498244535590231 ) ) ;
#851 = ADVANCED_FACE ( 'NONE', ( #5221 ), #6350, .T. ) ;
#852 = CARTESIAN_POINT ( 'NONE',  ( 59.30917539369505675, -13.12769224524051559, 293.5832628385307999 ) ) ;
#853 = CARTESIAN_POINT ( 'NONE',  ( -130.9868171408399462, -91.88282611735539263, 3.469446951953614189E-15 ) ) ;
#854 = VECTOR ( 'NONE', #363, 1000.000000000000114 ) ;
#855 = CARTESIAN_POINT ( 'NONE',  ( 134.6061912685151754, -66.19056267105210623, 4.133867502762946344 ) ) ;
#856 = DIRECTION ( 'NONE',  ( -1.000000000000000000, 0.000000000000000000, 0.000000000000000000 ) ) ;
#857 = DIRECTION ( 'NONE',  ( 0.9902903945359623483, 0.1390141521205945918, 0.000000000000000000 ) ) ;
#858 = VERTEX_POINT ( 'NONE', #1838 ) ;
#859 = VECTOR ( 'NONE', #3356, 1000.000000000000000 ) ;
#860 = EDGE_CURVE ( 'NONE', #1086, #5730, #18086, .T. ) ;
#861 = ORIENTED_EDGE ( 'NONE', *, *, #5577, .F. ) ;
#862 = CLOSED_SHELL ( 'NONE', ( #17922, #12414, #11863, #7855, #11249, #16008, #19643, #18744, #7325, #8273, #4630, #7416, #13850, #8626, #3371, #2282, #10782, #5475 ) ) ;
#863 = ORIENTED_EDGE ( 'NONE', *, *, #8888, .F. ) ;
#864 = EDGE_LOOP ( 'NONE', ( #14206, #12029, #8456, #17907 ) ) ;
#865 = AXIS2_PLACEMENT_3D ( 'NONE', #9927, #3687, #11837 ) ;
#866 = EDGE_LOOP ( 'NONE', ( #10462, #13743, #13664, #7998 ) ) ;
#867 = DIRECTION ( 'NONE',  ( -0.5300553768524375320, -0.8479630283625697595, 0.000000000000000000 ) ) ;
#868 = DIRECTION ( 'NONE',  ( -0.000000000000000000, -0.000000000000000000, 1.000000000000000000 ) ) ;
#869 = CARTESIAN_POINT ( 'NONE',  ( 62.95000000000000284, 0.000000000000000000, 5.035999999999999588 ) ) ;
#870 = VERTEX_POINT ( 'NONE', #12780 ) ;
#871 = ADVANCED_FACE ( 'NONE', ( #15659 ), #3279, .F. ) ;
#872 = DIRECTION ( 'NONE',  ( -0.000000000000000000, -0.000000000000000000, 1.000000000000000000 ) ) ;
#873 = CARTESIAN_POINT ( 'NONE',  ( 49.07263256785952166, -39.37628763770437956, 132.4711112102474146 ) ) ;
#874 = EDGE_CURVE ( 'NONE', #11852, #7829, #14215, .T. ) ;
#875 = ORIENTED_EDGE ( 'NONE', *, *, #149, .F. ) ;
#876 = DIRECTION ( 'NONE',  ( 1.000000000000000000, 0.000000000000000000, -0.000000000000000000 ) ) ;
#877 = DIRECTION ( 'NONE',  ( 0.1736481776669307198, -0.9848077530122080203, -0.000000000000000000 ) ) ;
#878 = DIRECTION ( 'NONE',  ( -1.000000000000000000, -3.491481338843133355E-15, 0.000000000000000000 ) ) ;
#879 = PLANE ( 'NONE',  #11470 ) ;
#880 = VECTOR ( 'NONE', #8878, 1000.000000000000114 ) ;
#881 = CARTESIAN_POINT ( 'NONE',  ( 4.189777606611760026E-13, -60.00000000000000000, -105.0000000000000142 ) ) ;
#882 = DIRECTION ( 'NONE',  ( -0.000000000000000000, -0.000000000000000000, -1.000000000000000000 ) ) ;
#883 = ORIENTED_EDGE ( 'NONE', *, *, #14292, .T. ) ;
#884 = EDGE_CURVE ( 'NONE', #6667, #10541, #9611, .T. ) ;
#885 = LINE ( 'NONE', #16552, #16463 ) ;
#886 = ORIENTED_EDGE ( 'NONE', *, *, #1081, .F. ) ;
#887 = ORIENTED_EDGE ( 'NONE', *, *, #9369, .T. ) ;
#888 = DIRECTION ( 'NONE',  ( -0.000000000000000000, -1.000000000000000000, -0.000000000000000000 ) ) ;
#889 = EDGE_LOOP ( 'NONE', ( #62, #9459, #3655, #15133 ) ) ;
#890 = ORIENTED_EDGE ( 'NONE', *, *, #13792, .T. ) ;
#891 = CIRCLE ( 'NONE', #13620, 3.224098631618461663 ) ;
#892 = CARTESIAN_POINT ( 'NONE',  ( -67.36461649554505016, 39.84224160888970800, 248.9926560891072143 ) ) ;
#893 = CIRCLE ( 'NONE', #19539, 15.91767397667354089 ) ;
#894 = CARTESIAN_POINT ( 'NONE',  ( -84.48076729319791411, -123.9477347680102639, 39.88981094656359971 ) ) ;
#895 = AXIS2_PLACEMENT_3D ( 'NONE', #13323, #2501, #8636 ) ;
#896 = EDGE_CURVE ( 'NONE', #12923, #1501, #465, .T. ) ;
#897 = FACE_OUTER_BOUND ( 'NONE', #6117, .T. ) ;
#898 = PLANE ( 'NONE',  #9640 ) ;
#899 = EDGE_CURVE ( 'NONE', #15648, #18566, #9811, .T. ) ;
#900 = ORIENTED_EDGE ( 'NONE', *, *, #1584, .T. ) ;
#901 = ADVANCED_FACE ( 'NONE', ( #16065 ), #3476, .F. ) ;
#902 = CARTESIAN_POINT ( 'NONE',  ( -134.6444961603440618, -66.11310837778573557, 35.67578572572296025 ) ) ;
#903 = CARTESIAN_POINT ( 'NONE',  ( 0.000000000000000000, 0.000000000000000000, 283.5832628385307999 ) ) ;
#904 = EDGE_CURVE ( 'NONE', #2440, #7038, #2047, .T. ) ;
#905 = CARTESIAN_POINT ( 'NONE',  ( 59.42266395395790823, -50.93469132750283279, 132.4711112102474146 ) ) ;
#906 = CARTESIAN_POINT ( 'NONE',  ( 57.92709869106709419, 18.28567271940532990, 293.5832628385307999 ) ) ;
#907 = ORIENTED_EDGE ( 'NONE', *, *, #964, .T. ) ;
#908 = DIRECTION ( 'NONE',  ( 6.982962677686266711E-15, -0.000000000000000000, 1.000000000000000000 ) ) ;
#909 = CARTESIAN_POINT ( 'NONE',  ( 82.17872144123518297, -125.4856950968007396, 7.470559115686841167 ) ) ;
#910 = DIRECTION ( 'NONE',  ( 0.1736481776669273336, 0.9848077530122085754, 0.000000000000000000 ) ) ;
#911 = VECTOR ( 'NONE', #6305, 1000.000000000000114 ) ;
#912 = VERTEX_POINT ( 'NONE', #10300 ) ;
#913 = CIRCLE ( 'NONE', #9421, 99.99999999999997158 ) ;
#914 = DIRECTION ( 'NONE',  ( 0.9902903945359623483, 0.1390141521205945918, 0.000000000000000000 ) ) ;
#915 = DIRECTION ( 'NONE',  ( -0.000000000000000000, -0.000000000000000000, 1.000000000000000000 ) ) ;
#916 = ORIENTED_EDGE ( 'NONE', *, *, #9093, .F. ) ;
#917 = ORIENTED_EDGE ( 'NONE', *, *, #11590, .T. ) ;
#918 = ORIENTED_EDGE ( 'NONE', *, *, #10465, .F. ) ;
#919 = CARTESIAN_POINT ( 'NONE',  ( -107.4999999999999716, -190.0000000000000000, 40.00000000000000000 ) ) ;
#920 = DIRECTION ( 'NONE',  ( 1.000000000000000000, 0.000000000000000000, 0.000000000000000000 ) ) ;
#921 = ORIENTED_EDGE ( 'NONE', *, *, #3637, .F. ) ;
#922 = AXIS2_PLACEMENT_3D ( 'NONE', #2246, #13164, #10012 ) ;
#923 = CARTESIAN_POINT ( 'NONE',  ( 96.59339607700708541, -114.7676973381603887, -9.527748193600634963 ) ) ;
#924 = DIRECTION ( 'NONE',  ( 1.000000000000000000, 0.000000000000000000, 0.000000000000000000 ) ) ;
#925 = AXIS2_PLACEMENT_3D ( 'NONE', #4318, #13517, #1146 ) ;
#926 = CIRCLE ( 'NONE', #13326, 62.91752772691707207 ) ;
#927 = AXIS2_PLACEMENT_3D ( 'NONE', #5331, #11563, #17816 ) ;
#928 = CARTESIAN_POINT ( 'NONE',  ( -86.48208760716207166, -122.5631135004756658, -3.009211076429890053 ) ) ;
#929 = CARTESIAN_POINT ( 'NONE',  ( 107.5000000000000284, -199.9999999999999716, 40.00000000000000000 ) ) ;
#930 = LINE ( 'NONE', #5643, #11229 ) ;
#931 = CARTESIAN_POINT ( 'NONE',  ( -20.01059462374426445, -13.41455640552162443, 14.88498244535559323 ) ) ;
#932 = CARTESIAN_POINT ( 'NONE',  ( -14.39940464655760799, -76.92888220842480962, 112.0427633081292385 ) ) ;
#933 = CARTESIAN_POINT ( 'NONE',  ( -139.8142396999972163, 1.712230611238718486E-14, -13.33333333333329307 ) ) ;
#934 = VERTEX_POINT ( 'NONE', #19618 ) ;
#935 = DIRECTION ( 'NONE',  ( 0.000000000000000000, 0.000000000000000000, -1.000000000000000000 ) ) ;
#936 = DIRECTION ( 'NONE',  ( -0.7660444431189770143, 0.6427876096865405842, 5.348151281215662765E-15 ) ) ;
#937 = VERTEX_POINT ( 'NONE', #7048 ) ;
#938 = AXIS2_PLACEMENT_3D ( 'NONE', #11223, #184, #17485 ) ;
#939 = AXIS2_PLACEMENT_3D ( 'NONE', #7315, #2621, #4246 ) ;
#940 = VECTOR ( 'NONE', #2427, 1000.000000000000000 ) ;
#941 = ORIENTED_EDGE ( 'NONE', *, *, #6979, .T. ) ;
#942 = ORIENTED_EDGE ( 'NONE', *, *, #18405, .T. ) ;
#943 = LINE ( 'NONE', #5760, #13587 ) ;
#944 = ORIENTED_EDGE ( 'NONE', *, *, #13641, .T. ) ;
#945 = DIRECTION ( 'NONE',  ( -0.5000000000000069944, 0.8660254037844344888, 0.000000000000000000 ) ) ;
#946 = LINE ( 'NONE', #10255, #14428 ) ;
#947 = DIRECTION ( 'NONE',  ( -0.000000000000000000, -0.000000000000000000, 1.000000000000000000 ) ) ;
#948 = CARTESIAN_POINT ( 'NONE',  ( -2.629322876227788264, -60.68773558783006905, 293.5832628385307999 ) ) ;
#949 = CIRCLE ( 'NONE', #5870, 15.91767397667354444 ) ;
#950 = AXIS2_PLACEMENT_3D ( 'NONE', #14173, #155, #18468 ) ;
#951 = ADVANCED_FACE ( 'NONE', ( #19331 ), #19432, .T. ) ;
#952 = PLANE ( 'NONE',  #2586 ) ;
#953 = DIRECTION ( 'NONE',  ( 0.000000000000000000, 0.000000000000000000, 1.000000000000000000 ) ) ;
#954 = CARTESIAN_POINT ( 'NONE',  ( 134.5971911056711292, -73.88063391573085426, 7.066933751406428321 ) ) ;
#955 = DIRECTION ( 'NONE',  ( -0.000000000000000000, -0.000000000000000000, 1.000000000000000000 ) ) ;
#956 = CYLINDRICAL_SURFACE ( 'NONE', #3822, 7.500000000000006217 ) ;
#957 = CARTESIAN_POINT ( 'NONE',  ( -51.23821591265114961, -28.63313560863453944, 132.4711112102474146 ) ) ;
#958 = ORIENTED_EDGE ( 'NONE', *, *, #5414, .T. ) ;
#959 = VERTEX_POINT ( 'NONE', #5412 ) ;
#960 = EDGE_CURVE ( 'NONE', #4825, #18093, #17397, .T. ) ;
#961 = VERTEX_POINT ( 'NONE', #17797 ) ;
#962 = AXIS2_PLACEMENT_3D ( 'NONE', #18141, #4121, #10352 ) ;
#963 = ORIENTED_EDGE ( 'NONE', *, *, #10639, .F. ) ;
#964 = EDGE_CURVE ( 'NONE', #10176, #13410, #4043, .T. ) ;
#965 = ORIENTED_EDGE ( 'NONE', *, *, #16251, .F. ) ;
#966 = CARTESIAN_POINT ( 'NONE',  ( 0.8220851292435327196, 58.69016442926522359, 132.4711112102474146 ) ) ;
#967 = CARTESIAN_POINT ( 'NONE',  ( 58.83691981461634413, -22.28973221005101735, 132.4711112102474146 ) ) ;
#968 = FACE_OUTER_BOUND ( 'NONE', #199, .T. ) ;
#969 = ORIENTED_EDGE ( 'NONE', *, *, #14026, .F. ) ;
#970 = CARTESIAN_POINT ( 'NONE',  ( 7.500000000000006217, 164.0736214083062805, 49.99999999999999289 ) ) ;
#971 = CARTESIAN_POINT ( 'NONE',  ( 0.000000000000000000, 0.000000000000000000, 293.5832628385307999 ) ) ;
#972 = ADVANCED_FACE ( 'NONE', ( #2343 ), #3769, .F. ) ;
#973 = ORIENTED_EDGE ( 'NONE', *, *, #19651, .F. ) ;
#974 = PLANE ( 'NONE',  #11706 ) ;
#975 = CIRCLE ( 'NONE', #5896, 150.0000000000000284 ) ;
#976 = CARTESIAN_POINT ( 'NONE',  ( 0.5584673446549194287, 9.967293815311103700, -0.7361406979141406071 ) ) ;
#977 = CARTESIAN_POINT ( 'NONE',  ( 71.18887634719571622, -147.8252249328912740, 39.99999999999999289 ) ) ;
#978 = VECTOR ( 'NONE', #19555, 1000.000000000000114 ) ;
#979 = AXIS2_PLACEMENT_3D ( 'NONE', #2375, #18027, #5444 ) ;
#980 = DIRECTION ( 'NONE',  ( -0.000000000000000000, -0.000000000000000000, 1.000000000000000000 ) ) ;
#981 = CARTESIAN_POINT ( 'NONE',  ( 112.4320812185962524, -22.51277856475483574, 14.88498244535466775 ) ) ;
#982 = DIRECTION ( 'NONE',  ( 0.9396926207859092051, -0.3420201433256662704, 0.000000000000000000 ) ) ;
#983 = ORIENTED_EDGE ( 'NONE', *, *, #5166, .F. ) ;
#984 = EDGE_CURVE ( 'NONE', #6115, #9946, #10014, .T. ) ;
#985 = CARTESIAN_POINT ( 'NONE',  ( 76.92888220842486646, -14.39940464655733976, 248.9926560891072143 ) ) ;
#986 = ORIENTED_EDGE ( 'NONE', *, *, #13979, .T. ) ;
#987 = EDGE_CURVE ( 'NONE', #11007, #1319, #6991, .T. ) ;
#988 = EDGE_LOOP ( 'NONE', ( #14488, #4292, #13951, #14059 ) ) ;
#989 = EDGE_CURVE ( 'NONE', #321, #1451, #11869, .T. ) ;
#990 = DIRECTION ( 'NONE',  ( -0.000000000000000000, -0.000000000000000000, 1.000000000000000000 ) ) ;
#991 = ORIENTED_EDGE ( 'NONE', *, *, #1968, .F. ) ;
#992 = ORIENTED_EDGE ( 'NONE', *, *, #14786, .F. ) ;
#993 = AXIS2_PLACEMENT_3D ( 'NONE', #10794, #3035, #4454 ) ;
#994 = LINE ( 'NONE', #7047, #13321 ) ;
#995 = DIRECTION ( 'NONE',  ( 0.6155349844899687950, -0.7881095627315619634, 0.000000000000000000 ) ) ;
#996 = FACE_OUTER_BOUND ( 'NONE', #16761, .T. ) ;
#997 = CARTESIAN_POINT ( 'NONE',  ( -38.41834839689332171, 68.18670162478844077, 110.9660488491356887 ) ) ;
#998 = VERTEX_POINT ( 'NONE', #10205 ) ;
#999 = EDGE_CURVE ( 'NONE', #17522, #8815, #1085, .T. ) ;
#1000 = FACE_OUTER_BOUND ( 'NONE', #8542, .T. ) ;
#1001 = FACE_OUTER_BOUND ( 'NONE', #11846, .T. ) ;
#1002 = CARTESIAN_POINT ( 'NONE',  ( 77.50000000000000000, 0.000000000000000000, -105.0000000000000142 ) ) ;
#1003 = CARTESIAN_POINT ( 'NONE',  ( -49.59485801383857506, -102.5175491340983882, 14.88498244535579929 ) ) ;
#1004 = VECTOR ( 'NONE', #8659, 1000.000000000000114 ) ;
#1005 = DIRECTION ( 'NONE',  ( -0.000000000000000000, -0.000000000000000000, 1.000000000000000000 ) ) ;
#1006 = DIRECTION ( 'NONE',  ( 0.1736481776669172583, 0.9848077530122103518, 0.000000000000000000 ) ) ;
#1007 = AXIS2_PLACEMENT_3D ( 'NONE', #5673, #3929, #11694 ) ;
#1008 = DIRECTION ( 'NONE',  ( -6.982962677686268288E-15, 3.944304526105059903E-31, -1.000000000000000000 ) ) ;
#1009 = ORIENTED_EDGE ( 'NONE', *, *, #7477, .F. ) ;
#1010 = LINE ( 'NONE', #19448, #1921 ) ;
#1011 = CYLINDRICAL_SURFACE ( 'NONE', #6981, 17.50000000000000355 ) ;
#1012 = EDGE_LOOP ( 'NONE', ( #5410, #2459 ) ) ;
#1013 = ADVANCED_FACE ( 'NONE', ( #13365 ), #20019, .F. ) ;
#1014 = EDGE_LOOP ( 'NONE', ( #1546, #3324, #12514, #214 ) ) ;
#1015 = EDGE_CURVE ( 'NONE', #3673, #7332, #3053, .T. ) ;
#1016 = ADVANCED_FACE ( 'NONE', ( #6021 ), #16749, .T. ) ;
#1017 = VECTOR ( 'NONE', #3317, 1000.000000000000000 ) ;
#1018 = FACE_OUTER_BOUND ( 'NONE', #6672, .T. ) ;
#1019 = DIRECTION ( 'NONE',  ( 0.3747554100459959958, 0.9271237148521535021, 0.000000000000000000 ) ) ;
#1020 = CARTESIAN_POINT ( 'NONE',  ( 5.485913980968211590, -1.678175111358135130, 293.5832628385307999 ) ) ;
#1021 = VERTEX_POINT ( 'NONE', #1409 ) ;
#1022 = DIRECTION ( 'NONE',  ( 1.000000000000000000, 0.000000000000000000, 0.000000000000000000 ) ) ;
#1023 = DIRECTION ( 'NONE',  ( -0.000000000000000000, -0.000000000000000000, 1.000000000000000000 ) ) ;
#1024 = CARTESIAN_POINT ( 'NONE',  ( 25.98398601615827985, 7.853099154550822192, 14.88498244535527171 ) ) ;
#1025 = FACE_OUTER_BOUND ( 'NONE', #18895, .T. ) ;
#1026 = PLANE ( 'NONE',  #15842 ) ;
#1027 = CARTESIAN_POINT ( 'NONE',  ( 0.000000000000000000, 0.000000000000000000, 248.9926560891072143 ) ) ;
#1028 = DIRECTION ( 'NONE',  ( -0.000000000000000000, -0.000000000000000000, 1.000000000000000000 ) ) ;
#1029 = CARTESIAN_POINT ( 'NONE',  ( 56.12662799072089115, -23.22641211976270270, 283.5832628385307999 ) ) ;
#1030 = ORIENTED_EDGE ( 'NONE', *, *, #1534, .T. ) ;
#1031 = FACE_OUTER_BOUND ( 'NONE', #3018, .T. ) ;
#1032 = DIRECTION ( 'NONE',  ( 0.000000000000000000, 0.000000000000000000, 1.000000000000000000 ) ) ;
#1033 = EDGE_CURVE ( 'NONE', #6085, #5634, #4169, .T. ) ;
#1034 = VERTEX_POINT ( 'NONE', #19814 ) ;
#1035 = ORIENTED_EDGE ( 'NONE', *, *, #16277, .T. ) ;
#1036 = AXIS2_PLACEMENT_3D ( 'NONE', #12711, #18869, #17440 ) ;
#1037 = ORIENTED_EDGE ( 'NONE', *, *, #15249, .T. ) ;
#1038 = ADVANCED_FACE ( 'NONE', ( #10705 ), #15108, .T. ) ;
#1039 = DIRECTION ( 'NONE',  ( -1.000000000000000000, 0.000000000000000000, 0.000000000000000000 ) ) ;
#1040 = ORIENTED_EDGE ( 'NONE', *, *, #237, .F. ) ;
#1041 = CARTESIAN_POINT ( 'NONE',  ( 0.000000000000000000, 0.000000000000000000, -49.99999999999999289 ) ) ;
#1042 = DIRECTION ( 'NONE',  ( 0.9396926207859093161, -0.3420201433256663259, 0.000000000000000000 ) ) ;
#1043 = DIRECTION ( 'NONE',  ( -0.9749279121818226201, -0.2225209339563185285, 0.000000000000000000 ) ) ;
#1044 = CARTESIAN_POINT ( 'NONE',  ( -19.30071112029641967, 55.43188410062188609, 132.4711112102474146 ) ) ;
#1045 = ORIENTED_EDGE ( 'NONE', *, *, #5358, .T. ) ;
#1046 = FACE_OUTER_BOUND ( 'NONE', #12800, .T. ) ;
#1047 = CARTESIAN_POINT ( 'NONE',  ( -127.6186898578139477, -78.88112642940109254, -0.7766205772862178058 ) ) ;
#1048 = CARTESIAN_POINT ( 'NONE',  ( 131.2702496982006153, -90.86622748989321963, -2.335466277633964500E-16 ) ) ;
#1049 = AXIS2_PLACEMENT_3D ( 'NONE', #3014, #142, #17237 ) ;
#1050 = DIRECTION ( 'NONE',  ( 1.000000000000000000, 0.000000000000000000, 0.000000000000000000 ) ) ;
#1051 = DIRECTION ( 'NONE',  ( 6.982962677686266711E-15, -0.000000000000000000, 1.000000000000000000 ) ) ;
#1052 = CARTESIAN_POINT ( 'NONE',  ( -133.2712073786778433, -68.96827650415615096, 31.07541976963426578 ) ) ;
#1053 = ORIENTED_EDGE ( 'NONE', *, *, #2363, .T. ) ;
#1054 = MANIFOLD_SOLID_BREP ( 'Fillet3', #7080 ) ;
#1055 = CARTESIAN_POINT ( 'NONE',  ( 19.23614321207236699, -57.61627707419557964, 283.5832628385307999 ) ) ;
#1056 = CIRCLE ( 'NONE', #8250, 3.224098631618458555 ) ;
#1057 = ORIENTED_EDGE ( 'NONE', *, *, #1482, .T. ) ;
#1058 = ORIENTED_EDGE ( 'NONE', *, *, #376, .F. ) ;
#1059 = VERTEX_POINT ( 'NONE', #16959 ) ;
#1060 = CIRCLE ( 'NONE', #5338, 27.50000000000000355 ) ;
#1061 = ORIENTED_EDGE ( 'NONE', *, *, #13864, .F. ) ;
#1062 = DIRECTION ( 'NONE',  ( -0.2080686897406911207, -0.9781142164131917394, 0.000000000000000000 ) ) ;
#1063 = DIRECTION ( 'NONE',  ( 1.000000000000000000, 0.000000000000000000, 0.000000000000000000 ) ) ;
#1064 = ORIENTED_EDGE ( 'NONE', *, *, #6051, .F. ) ;
#1065 = AXIS2_PLACEMENT_3D ( 'NONE', #69, #12331, #10906 ) ;
#1066 = DIRECTION ( 'NONE',  ( -1.000000000000000000, 0.000000000000000000, 0.000000000000000000 ) ) ;
#1067 = CARTESIAN_POINT ( 'NONE',  ( -49.59485801383857506, -102.5175491340983882, 14.88498244535579929 ) ) ;
#1068 = ORIENTED_EDGE ( 'NONE', *, *, #13216, .T. ) ;
#1069 = LINE ( 'NONE', #4050, #15986 ) ;
#1070 = CARTESIAN_POINT ( 'NONE',  ( 120.7779226595531128, 102.2982297021113141, 39.99999999999999289 ) ) ;
#1071 = CARTESIAN_POINT ( 'NONE',  ( -42.50000000000000000, 5.204748896376250896E-15, -100.0000000000000000 ) ) ;
#1072 = FACE_OUTER_BOUND ( 'NONE', #19255, .T. ) ;
#1073 = UNCERTAINTY_MEASURE_WITH_UNIT (LENGTH_MEASURE( 1.000000000000000082E-05 ), #7638, 'distance_accuracy_value', 'NONE');
#1074 = VECTOR ( 'NONE', #12151, 1000.000000000000114 ) ;
#1075 = CARTESIAN_POINT ( 'NONE',  ( 130.6671641404130639, -73.67117004795007063, 45.70932628007447107 ) ) ;
#1076 = FACE_OUTER_BOUND ( 'NONE', #1916, .T. ) ;
#1077 = ORIENTED_EDGE ( 'NONE', *, *, #6165, .F. ) ;
#1078 = ORIENTED_EDGE ( 'NONE', *, *, #10747, .F. ) ;
#1079 = CIRCLE ( 'NONE', #19402, 3.224098631618458999 ) ;
#1080 = VERTEX_POINT ( 'NONE', #12131 ) ;
#1081 = EDGE_CURVE ( 'NONE', #5634, #13285, #6344, .T. ) ;
#1082 = DIRECTION ( 'NONE',  ( 0.000000000000000000, 0.000000000000000000, 1.000000000000000000 ) ) ;
#1083 = EDGE_CURVE ( 'NONE', #7829, #10900, #7741, .T. ) ;
#1084 = MANIFOLD_SOLID_BREP ( 'Boss-Extrude13', #11640 ) ;
#1085 = CIRCLE ( 'NONE', #9280, 60.74260934110282051 ) ;
#1086 = VERTEX_POINT ( 'NONE', #8151 ) ;
#1087 = ORIENTED_EDGE ( 'NONE', *, *, #9983, .T. ) ;
#1088 = CARTESIAN_POINT ( 'NONE',  ( 71.18887634719571622, -147.8252249328912740, 60.00000000000000000 ) ) ;
#1089 = CYLINDRICAL_SURFACE ( 'NONE', #11995, 60.74260934110282051 ) ;
#1090 = ORIENTED_EDGE ( 'NONE', *, *, #6919, .F. ) ;
#1091 = CARTESIAN_POINT ( 'NONE',  ( -42.50000000000000000, 5.204748896376250896E-15, -100.0000000000000000 ) ) ;
#1092 = CARTESIAN_POINT ( 'NONE',  ( 148.9554720520395392, -17.67108784863215476, 60.00000000000000000 ) ) ;
#1093 = ORIENTED_EDGE ( 'NONE', *, *, #4109, .F. ) ;
#1094 = EDGE_CURVE ( 'NONE', #541, #1941, #19405, .T. ) ;
#1095 = DIRECTION ( 'NONE',  ( 1.000000000000000000, 0.000000000000000000, 0.000000000000000000 ) ) ;
#1096 = DIRECTION ( 'NONE',  ( -0.000000000000000000, -1.000000000000000000, -0.000000000000000000 ) ) ;
#1097 = EDGE_CURVE ( 'NONE', #12671, #18381, #3555, .T. ) ;
#1098 = AXIS2_PLACEMENT_3D ( 'NONE', #19361, #16095, #3508 ) ;
#1099 = EDGE_CURVE ( 'NONE', #16204, #18358, #3152, .T. ) ;
#1100 = CARTESIAN_POINT ( 'NONE',  ( 0.000000000000000000, 0.000000000000000000, -10.00000000000000178 ) ) ;
#1101 = ORIENTED_EDGE ( 'NONE', *, *, #14424, .T. ) ;
#1102 = AXIS2_PLACEMENT_3D ( 'NONE', #13954, #20197, #153 ) ;
#1103 = CARTESIAN_POINT ( 'NONE',  ( 48.17797692984161984, 36.99387960884179449, 283.5832628385307999 ) ) ;
#1104 = CARTESIAN_POINT ( 'NONE',  ( -133.3655458879726723, -81.62736142943097661, 38.20259313401145107 ) ) ;
#1105 = PLANE ( 'NONE',  #9572 ) ;
#1106 = ORIENTED_EDGE ( 'NONE', *, *, #7531, .F. ) ;
#1107 = CARTESIAN_POINT ( 'NONE',  ( 71.18887634719571622, -147.8252249328912740, 60.00000000000000000 ) ) ;
#1108 = CARTESIAN_POINT ( 'NONE',  ( 133.2435246741110006, -68.89240257401093004, 10.00000000000000178 ) ) ;
#1109 = ORIENTED_EDGE ( 'NONE', *, *, #3534, .T. ) ;
#1110 = ORIENTED_EDGE ( 'NONE', *, *, #2464, .F. ) ;
#1111 = EDGE_CURVE ( 'NONE', #10388, #2638, #12548, .T. ) ;
#1112 = DIRECTION ( 'NONE',  ( -0.000000000000000000, -0.000000000000000000, 1.000000000000000000 ) ) ;
#1113 =( GEOMETRIC_REPRESENTATION_CONTEXT ( 3 ) GLOBAL_UNCERTAINTY_ASSIGNED_CONTEXT ( ( #10482 ) ) GLOBAL_UNIT_ASSIGNED_CONTEXT ( ( #20157, #10630, #1338 ) ) REPRESENTATION_CONTEXT ( 'NONE', 'WORKASPACE' ) );
#1114 = VERTEX_POINT ( 'NONE', #14495 ) ;
#1115 = DIRECTION ( 'NONE',  ( 1.000000000000000000, 0.000000000000000000, -0.000000000000000000 ) ) ;
#1116 = DIRECTION ( 'NONE',  ( -0.9993852124581887875, 0.03505990758545545621, 0.000000000000000000 ) ) ;
#1117 = AXIS2_PLACEMENT_3D ( 'NONE', #16706, #4119, #16807 ) ;
#1118 = EDGE_LOOP ( 'NONE', ( #11292, #9512, #14988, #2323 ) ) ;
#1119 = CARTESIAN_POINT ( 'NONE',  ( 20.84572577951164618, 54.86954475316263569, 132.4711112102474146 ) ) ;
#1120 = DIRECTION ( 'NONE',  ( -0.000000000000000000, -0.000000000000000000, 1.000000000000000000 ) ) ;
#1121 = EDGE_CURVE ( 'NONE', #19010, #5530, #7843, .T. ) ;
#1122 = ADVANCED_FACE ( 'NONE', ( #11215 ), #16037, .T. ) ;
#1123 = EDGE_CURVE ( 'NONE', #2923, #13175, #17579, .T. ) ;
#1124 = CARTESIAN_POINT ( 'NONE',  ( -138.0190090189069849, -24.44405553796960717, -9.999999999999987566 ) ) ;
#1125 = FACE_OUTER_BOUND ( 'NONE', #123, .T. ) ;
#1126 = CARTESIAN_POINT ( 'NONE',  ( 7.500000000000420997, -60.00000000000000000, -115.0000000000000000 ) ) ;
#1127 = ADVANCED_FACE ( 'NONE', ( #14298 ), #279, .T. ) ;
#1128 = FACE_OUTER_BOUND ( 'NONE', #10179, .T. ) ;
#1129 = TOROIDAL_SURFACE ( 'NONE', #3753, 160.0000000000000284, 10.00000000000000000 ) ;
#1130 = DIRECTION ( 'NONE',  ( 0.7660444431189835646, -0.6427876096865328126, 0.000000000000000000 ) ) ;
#1131 = CARTESIAN_POINT ( 'NONE',  ( -141.8714406926361278, -48.70825716237271763, 49.99999999999999289 ) ) ;
#1132 = LINE ( 'NONE', #4304, #3995 ) ;
#1133 = ORIENTED_EDGE ( 'NONE', *, *, #5414, .F. ) ;
#1134 = CARTESIAN_POINT ( 'NONE',  ( -2.647132857508548209, -114.6332882433608376, 14.88498244535546888 ) ) ;
#1135 = FACE_OUTER_BOUND ( 'NONE', #17367, .T. ) ;
#1136 = ORIENTED_EDGE ( 'NONE', *, *, #18917, .F. ) ;
#1137 = ORIENTED_EDGE ( 'NONE', *, *, #1083, .F. ) ;
#1138 = EDGE_CURVE ( 'NONE', #15303, #5586, #6629, .T. ) ;
#1139 =( NAMED_UNIT ( * ) SI_UNIT ( $, .STERADIAN. ) SOLID_ANGLE_UNIT ( ) );
#1140 = AXIS2_PLACEMENT_3D ( 'NONE', #7543, #13678, #10302 ) ;
#1141 = EDGE_LOOP ( 'NONE', ( #1644, #11755 ) ) ;
#1142 = DIRECTION ( 'NONE',  ( 1.000000000000000000, 0.000000000000000000, 0.000000000000000000 ) ) ;
#1143 = ORIENTED_EDGE ( 'NONE', *, *, #23, .T. ) ;
#1144 = CARTESIAN_POINT ( 'NONE',  ( 131.4993367897275220, -89.99660315853893167, 0.04843323613514682879 ) ) ;
#1145 = DIRECTION ( 'NONE',  ( -0.000000000000000000, -0.000000000000000000, 1.000000000000000000 ) ) ;
#1146 = DIRECTION ( 'NONE',  ( 1.000000000000000000, 0.000000000000000000, 0.000000000000000000 ) ) ;
#1147 = EDGE_CURVE ( 'NONE', #16478, #13051, #12872, .T. ) ;
#1148 = CARTESIAN_POINT ( 'NONE',  ( -12.14957802882752524, -59.51724408343569905, 283.5832628385307999 ) ) ;
#1149 = CARTESIAN_POINT ( 'NONE',  ( 5.111158570922254896, -2.605298826210304064, 283.5832628385307999 ) ) ;
#1150 = AXIS2_PLACEMENT_3D ( 'NONE', #10589, #13768, #9061 ) ;
#1151 = VERTEX_POINT ( 'NONE', #3451 ) ;
#1152 = DIRECTION ( 'NONE',  ( -0.000000000000000000, -1.000000000000000000, -0.000000000000000000 ) ) ;
#1153 = CARTESIAN_POINT ( 'NONE',  ( -130.7712900376313598, -73.57687123476972602, 1.577274671842293197 ) ) ;
#1154 = CARTESIAN_POINT ( 'NONE',  ( 129.2715203052800632, -76.16417937455307197, 0.08780702205603270472 ) ) ;
#1155 = DIRECTION ( 'NONE',  ( -1.000000000000000000, 0.000000000000000000, 0.000000000000000000 ) ) ;
#1156 = DIRECTION ( 'NONE',  ( -0.000000000000000000, -0.000000000000000000, 1.000000000000000000 ) ) ;
#1157 = LINE ( 'NONE', #7207, #5085 ) ;
#1158 = ADVANCED_FACE ( 'NONE', ( #10912 ), #12853, .F. ) ;
#1159 = ORIENTED_EDGE ( 'NONE', *, *, #15092, .T. ) ;
#1160 = PLANE ( 'NONE',  #3024 ) ;
#1161 = ORIENTED_EDGE ( 'NONE', *, *, #1765, .F. ) ;
#1162 = ORIENTED_EDGE ( 'NONE', *, *, #10042, .F. ) ;
#1163 = VECTOR ( 'NONE', #5970, 1000.000000000000000 ) ;
#1164 = ORIENTED_EDGE ( 'NONE', *, *, #4048, .F. ) ;
#1165 = ORIENTED_EDGE ( 'NONE', *, *, #5833, .F. ) ;
#1166 = CARTESIAN_POINT ( 'NONE',  ( 13.12726406102079224, 59.30716253403178939, 293.5832628385307999 ) ) ;
#1167 = CARTESIAN_POINT ( 'NONE',  ( 0.8220851292435327196, 78.26059000578311498, 112.7772637782949943 ) ) ;
#1168 = EDGE_LOOP ( 'NONE', ( #17349, #1613 ) ) ;
#1169 = CARTESIAN_POINT ( 'NONE',  ( 0.000000000000000000, 0.000000000000000000, 293.5832628385307999 ) ) ;
#1170 = DIRECTION ( 'NONE',  ( 1.000000000000000000, 0.000000000000000000, -6.977185866873308817E-15 ) ) ;
#1171 = ORIENTED_EDGE ( 'NONE', *, *, #13037, .F. ) ;
#1172 = CARTESIAN_POINT ( 'NONE',  ( -79.44021699520564539, 115.2109178599716017, -12.09771328782125899 ) ) ;
#1173 = DIRECTION ( 'NONE',  ( 0.000000000000000000, 0.000000000000000000, -1.000000000000000000 ) ) ;
#1174 = CYLINDRICAL_SURFACE ( 'NONE', #13335, 7.500000000000020428 ) ;
#1175 = LINE ( 'NONE', #14995, #6259 ) ;
#1176 = VECTOR ( 'NONE', #16733, 1000.000000000000000 ) ;
#1177 = AXIS2_PLACEMENT_3D ( 'NONE', #18806, #275, #4789 ) ;
#1178 = CARTESIAN_POINT ( 'NONE',  ( 125.5756761630927372, -82.07265954316353884, 41.04722885697084678 ) ) ;
#1179 = CARTESIAN_POINT ( 'NONE',  ( -176.7850001792985495, -194.3449193228699698, 37.50924103860242553 ) ) ;
#1180 = ORIENTED_EDGE ( 'NONE', *, *, #18056, .F. ) ;
#1181 = AXIS2_PLACEMENT_3D ( 'NONE', #18694, #7526, #4675 ) ;
#1182 = CARTESIAN_POINT ( 'NONE',  ( 166.7850001792985495, -189.9999999999999432, 40.00000000000000000 ) ) ;
#1183 = ORIENTED_EDGE ( 'NONE', *, *, #97, .F. ) ;
#1184 = ORIENTED_EDGE ( 'NONE', *, *, #5153, .T. ) ;
#1185 = DIRECTION ( 'NONE',  ( 0.000000000000000000, 0.000000000000000000, -1.000000000000000000 ) ) ;
#1186 = MANIFOLD_SOLID_BREP ( 'Chamfer1', #7388 ) ;
#1187 = VERTEX_POINT ( 'NONE', #19014 ) ;
#1188 = ORIENTED_EDGE ( 'NONE', *, *, #12282, .T. ) ;
#1189 = AXIS2_PLACEMENT_3D ( 'NONE', #2625, #2520, #15088 ) ;
#1190 = LINE ( 'NONE', #5606, #6171 ) ;
#1191 = VECTOR ( 'NONE', #16387, 1000.000000000000000 ) ;
#1192 = FILL_AREA_STYLE ('',( #15207 ) ) ;
#1193 = CARTESIAN_POINT ( 'NONE',  ( -29.99999999999887379, 275.0000000000000000, 4.999999999999158007 ) ) ;
#1194 = ORIENTED_EDGE ( 'NONE', *, *, #4603, .T. ) ;
#1195 = LINE ( 'NONE', #13780, #11300 ) ;
#1196 = DIRECTION ( 'NONE',  ( -0.000000000000000000, -0.000000000000000000, 1.000000000000000000 ) ) ;
#1197 = ORIENTED_EDGE ( 'NONE', *, *, #7928, .T. ) ;
#1198 = CIRCLE ( 'NONE', #19820, 3.224098631618463440 ) ;
#1199 = CARTESIAN_POINT ( 'NONE',  ( -81.46657151846173406, 123.3484521904389339, -23.05424169220087904 ) ) ;
#1200 = DIRECTION ( 'NONE',  ( 1.000000000000000000, 0.000000000000000000, -6.994638739193269649E-15 ) ) ;
#1201 = EDGE_CURVE ( 'NONE', #10024, #16800, #75, .T. ) ;
#1202 = FACE_OUTER_BOUND ( 'NONE', #10914, .T. ) ;
#1203 = VERTEX_POINT ( 'NONE', #13139 ) ;
#1204 = CARTESIAN_POINT ( 'NONE',  ( 51.24245927909996112, -32.62092819947974220, 293.5832628385307999 ) ) ;
#1205 = CARTESIAN_POINT ( 'NONE',  ( 51.24245927909996112, -32.62092819947974220, 283.5832628385307999 ) ) ;
#1206 = CARTESIAN_POINT ( 'NONE',  ( -85.14505921096956342, 111.1339209219067925, 29.65373415551709968 ) ) ;
#1207 = ORIENTED_EDGE ( 'NONE', *, *, #3241, .F. ) ;
#1208 = B_SPLINE_CURVE_WITH_KNOTS ( 'NONE', 3,
 ( #15433, #8979, #12353, #15220, #7254, #3065, #19929, #18612, #6135, #18505, #13892, #20036, #16866, #10412, #12250, #4486, #5722, #2657, #1317, #1104, #19826, #11936, #15026, #9189, #5822, #7653, #1424, #19726 ),
 .UNSPECIFIED., .F., .F.,
 ( 4, 2, 2, 2, 2, 2, 2, 2, 2, 2, 2, 2, 2, 4 ),
 ( 0.000000000000000000, 0.001466376146900913230, 0.002199564220351372772, 0.002932752293801832531, 0.004399128440702757686, 0.005865504587603682408, 0.007331880734504607131, 0.008798256881405530985, 0.01026463302830645831, 0.01173100917520738216, 0.01466376146900919344, 0.01759651376281100299, 0.02052926605661281600, 0.02346201835041462902 ),
 .UNSPECIFIED. ) ;
#1209 = CARTESIAN_POINT ( 'NONE',  ( -1.396592535537253342E-14, 0.000000000000000000, 39.88498244535545467 ) ) ;
#1210 = CARTESIAN_POINT ( 'NONE',  ( -73.25972925305609351, 27.53920554013712874, 132.4711112102474146 ) ) ;
#1211 = ORIENTED_EDGE ( 'NONE', *, *, #9158, .T. ) ;
#1212 =( REPRESENTATION_RELATIONSHIP ('NONE','NONE', #17382, #6269 ) REPRESENTATION_RELATIONSHIP_WITH_TRANSFORMATION ( #2072 )SHAPE_REPRESENTATION_RELATIONSHIP( ) );
#1213 = VERTEX_POINT ( 'NONE', #19208 ) ;
#1214 = CARTESIAN_POINT ( 'NONE',  ( -82.18707601317574074, -125.4802243595265736, 32.59999595717800247 ) ) ;
#1215 = AXIS2_PLACEMENT_3D ( 'NONE', #17388, #3363, #5010 ) ;
#1216 = ADVANCED_FACE ( 'NONE', ( #5483 ), #2122, .F. ) ;
#1217 = CIRCLE ( 'NONE', #4496, 7.500000000000002665 ) ;
#1218 = EDGE_CURVE ( 'NONE', #8668, #14953, #17771, .T. ) ;
#1219 = EDGE_LOOP ( 'NONE', ( #8699, #14779, #11738, #17366 ) ) ;
#1220 = ADVANCED_FACE ( 'NONE', ( #16437, #9987, #19404, #7021, #5198, #11707 ), #5387, .T. ) ;
#1221 = PLANE ( 'NONE',  #11085 ) ;
#1222 = CARTESIAN_POINT ( 'NONE',  ( -150.0000000000000284, 0.000000000000000000, 60.00000000000000000 ) ) ;
#1223 = ORIENTED_EDGE ( 'NONE', *, *, #14398, .T. ) ;
#1224 = CARTESIAN_POINT ( 'NONE',  ( 97.50000000000000000, -115.4778303846449887, 10.00000000000000355 ) ) ;
#1225 = DIRECTION ( 'NONE',  ( 0.9396926207859057634, -0.3420201433256758183, -6.456589605409169860E-15 ) ) ;
#1226 = CIRCLE ( 'NONE', #9067, 60.74260934110282051 ) ;
#1227 = ADVANCED_FACE ( 'NONE', ( #11615 ), #14692, .F. ) ;
#1228 = CARTESIAN_POINT ( 'NONE',  ( -134.7445384735268590, -31.41486127453163490, -19.78846255602397619 ) ) ;
#1229 = PLANE ( 'NONE',  #2766 ) ;
#1230 = CIRCLE ( 'NONE', #13637, 7.500000000000001776 ) ;
#1231 = DIRECTION ( 'NONE',  ( 0.000000000000000000, 0.000000000000000000, -1.000000000000000000 ) ) ;
#1232 = CARTESIAN_POINT ( 'NONE',  ( 0.000000000000000000, -3.004629197474327134E-15, 9.000000000000000000 ) ) ;
#1233 = LINE ( 'NONE', #18432, #11402 ) ;
#1234 = CARTESIAN_POINT ( 'NONE',  ( 95.87737486567891665, -116.0928213521003727, 30.55387713521830761 ) ) ;
#1235 = ORIENTED_EDGE ( 'NONE', *, *, #20238, .T. ) ;
#1236 = CYLINDRICAL_SURFACE ( 'NONE', #15630, 112.8770930172170210 ) ;
#1237 = CARTESIAN_POINT ( 'NONE',  ( -23.22718332831480481, -56.12853591711337486, 293.5832628385307999 ) ) ;
#1238 = VERTEX_POINT ( 'NONE', #14592 ) ;
#1239 = ORIENTED_EDGE ( 'NONE', *, *, #8863, .T. ) ;
#1240 = SHAPE_REPRESENTATION_RELATIONSHIP ( 'NONE' , 'NONE' ,  #6269, #19668 ) ;
#1241 = ADVANCED_FACE ( 'NONE', ( #13235 ), #3941, .F. ) ;
#1242 = CIRCLE ( 'NONE', #18624, 15.91767397667355510 ) ;
#1243 = EDGE_CURVE ( 'NONE', #1901, #16780, #3744, .T. ) ;
#1244 = AXIS2_PLACEMENT_3D ( 'NONE', #14765, #2203, #19186 ) ;
#1245 = ORIENTED_EDGE ( 'NONE', *, *, #7902, .F. ) ;
#1246 = ADVANCED_FACE ( 'NONE', ( #16335 ), #2419, .F. ) ;
#1247 = AXIS2_PLACEMENT_3D ( 'NONE', #7167, #11750, #11657 ) ;
#1248 = FACE_BOUND ( 'NONE', #5298, .T. ) ;
#1249 = EDGE_LOOP ( 'NONE', ( #14006, #18841 ) ) ;
#1250 = FACE_OUTER_BOUND ( 'NONE', #9273, .T. ) ;
#1251 = DIRECTION ( 'NONE',  ( -0.7660444431189707970, -0.6427876096865481337, 0.000000000000000000 ) ) ;
#1252 = PLANE ( 'NONE',  #7327 ) ;
#1253 = CARTESIAN_POINT ( 'NONE',  ( -100.0290433905560974, -111.7820284657242951, 39.61898166952727962 ) ) ;
#1254 = DIRECTION ( 'NONE',  ( 6.982962677686266711E-15, 0.000000000000000000, 1.000000000000000000 ) ) ;
#1255 = FACE_OUTER_BOUND ( 'NONE', #10175, .T. ) ;
#1256 = ORIENTED_EDGE ( 'NONE', *, *, #7505, .F. ) ;
#1257 = CARTESIAN_POINT ( 'NONE',  ( 141.8714406926368099, -48.70825716237082759, 60.00000000000000000 ) ) ;
#1258 = CARTESIAN_POINT ( 'NONE',  ( -134.4925794577901002, -74.66012650512811888, 6.056824688956695013 ) ) ;
#1259 = EDGE_CURVE ( 'NONE', #7835, #16054, #5293, .T. ) ;
#1260 = CARTESIAN_POINT ( 'NONE',  ( 133.6471402512195255, -68.10643054410130048, 0.2438139681274874293 ) ) ;
#1261 = CIRCLE ( 'NONE', #14662, 106.4288957539801004 ) ;
#1262 = DIRECTION ( 'NONE',  ( 1.000000000000000000, 0.000000000000000000, 0.000000000000000000 ) ) ;
#1263 = CARTESIAN_POINT ( 'NONE',  ( -110.0000000000000142, 0.000000000000000000, 5.000000000000000888 ) ) ;
#1264 = AXIS2_PLACEMENT_3D ( 'NONE', #6211, #1494, #1695 ) ;
#1265 = DIRECTION ( 'NONE',  ( -1.613511099790691498E-16, 1.000000000000000000, 0.000000000000000000 ) ) ;
#1266 = VECTOR ( 'NONE', #16070, 1000.000000000000000 ) ;
#1267 = ORIENTED_EDGE ( 'NONE', *, *, #13772, .F. ) ;
#1268 = AXIS2_PLACEMENT_3D ( 'NONE', #8457, #16834, #9263 ) ;
#1269 = CARTESIAN_POINT ( 'NONE',  ( 5.281164089014827923, 2.240720816136096083, 293.5832628385307999 ) ) ;
#1270 = VERTEX_POINT ( 'NONE', #8648 ) ;
#1271 = EDGE_CURVE ( 'NONE', #7556, #3875, #679, .T. ) ;
#1272 = EDGE_CURVE ( 'NONE', #19563, #3694, #14883, .T. ) ;
#1273 = EDGE_CURVE ( 'NONE', #14920, #11567, #3842, .T. ) ;
#1274 = VERTEX_POINT ( 'NONE', #7120 ) ;
#1275 = AXIS2_PLACEMENT_3D ( 'NONE', #8417, #2288, #19366 ) ;
#1276 = EDGE_CURVE ( 'NONE', #9351, #9578, #12949, .T. ) ;
#1277 = EDGE_LOOP ( 'NONE', ( #20096, #14289, #14387, #19517 ) ) ;
#1278 = CONICAL_SURFACE ( 'NONE', #8779, 9.000000000000000000, 1.047197551196600296 ) ;
#1279 = DIRECTION ( 'NONE',  ( -0.6718749999999997780, 0.7406645559057084549, 0.000000000000000000 ) ) ;
#1280 = AXIS2_PLACEMENT_3D ( 'NONE', #7644, #4795, #12243 ) ;
#1281 = CARTESIAN_POINT ( 'NONE',  ( 59.51724408343574879, -12.14957802882732452, 293.5832628385307999 ) ) ;
#1282 = CARTESIAN_POINT ( 'NONE',  ( 53.78543575132128751, 32.64570716507559922, 248.9926560891072143 ) ) ;
#1283 = ORIENTED_EDGE ( 'NONE', *, *, #13160, .T. ) ;
#1284 = CARTESIAN_POINT ( 'NONE',  ( 170.2125097089226244, -199.3942630591406839, 0.000000000000000000 ) ) ;
#1285 = PLANE ( 'NONE',  #17322 ) ;
#1286 = EDGE_LOOP ( 'NONE', ( #9182, #2764 ) ) ;
#1287 = DIRECTION ( 'NONE',  ( 1.000000000000000000, 0.000000000000000000, 0.000000000000000000 ) ) ;
#1288 = LINE ( 'NONE', #13756, #1176 ) ;
#1289 = DIRECTION ( 'NONE',  ( -0.000000000000000000, -0.000000000000000000, -1.000000000000000000 ) ) ;
#1290 = CARTESIAN_POINT ( 'NONE',  ( 27.50000000000001776, 3.367778697655222096E-15, 49.99999999999998579 ) ) ;
#1291 = UNCERTAINTY_MEASURE_WITH_UNIT (LENGTH_MEASURE( 1.000000000000000082E-05 ), #18131, 'distance_accuracy_value', 'NONE');
#1292 = CARTESIAN_POINT ( 'NONE',  ( 9.381844291199747943, -57.94128254008187184, 132.4711112102474146 ) ) ;
#1293 = DIRECTION ( 'NONE',  ( 0.6427876096865404731, -0.7660444431189771253, 0.000000000000000000 ) ) ;
#1294 = CIRCLE ( 'NONE', #12387, 15.91767397667355510 ) ;
#1295 = VECTOR ( 'NONE', #19771, 1000.000000000000114 ) ;
#1296 = ORIENTED_EDGE ( 'NONE', *, *, #6018, .F. ) ;
#1297 = EDGE_LOOP ( 'NONE', ( #8065, #1927, #6457, #944 ) ) ;
#1298 = CARTESIAN_POINT ( 'NONE',  ( 0.000000000000000000, 0.000000000000000000, 283.5832628385307999 ) ) ;
#1299 = ORIENTED_EDGE ( 'NONE', *, *, #10082, .F. ) ;
#1300 = VERTEX_POINT ( 'NONE', #5580 ) ;
#1301 = DIRECTION ( 'NONE',  ( 6.982962677686266711E-15, -0.000000000000000000, 1.000000000000000000 ) ) ;
#1302 = VERTEX_POINT ( 'NONE', #11799 ) ;
#1303 = VERTEX_POINT ( 'NONE', #18065 ) ;
#1304 = EDGE_CURVE ( 'NONE', #6273, #295, #16535, .T. ) ;
#1305 = FACE_BOUND ( 'NONE', #15828, .T. ) ;
#1306 =( GEOMETRIC_REPRESENTATION_CONTEXT ( 3 ) GLOBAL_UNCERTAINTY_ASSIGNED_CONTEXT ( ( #18710 ) ) GLOBAL_UNIT_ASSIGNED_CONTEXT ( ( #14131, #18961, #120 ) ) REPRESENTATION_CONTEXT ( 'NONE', 'WORKASPACE' ) );
#1307 = CYLINDRICAL_SURFACE ( 'NONE', #14633, 17.50000000000000355 ) ;
#1308 = ORIENTED_EDGE ( 'NONE', *, *, #4869, .T. ) ;
#1309 = AXIS2_PLACEMENT_3D ( 'NONE', #17020, #1571, #5973 ) ;
#1310 = FACE_OUTER_BOUND ( 'NONE', #18191, .T. ) ;
#1311 = LINE ( 'NONE', #8969, #8332 ) ;
#1312 = ORIENTED_EDGE ( 'NONE', *, *, #4808, .T. ) ;
#1313 = CARTESIAN_POINT ( 'NONE',  ( -75.15677698908424986, 129.5154647000477723, -14.68683001631521989 ) ) ;
#1314 = FACE_OUTER_BOUND ( 'NONE', #4391, .T. ) ;
#1315 = DIRECTION ( 'NONE',  ( 0.6427876096865353661, 0.7660444431189813441, 0.000000000000000000 ) ) ;
#1316 = CARTESIAN_POINT ( 'NONE',  ( -27.49999999999998934, 0.000000000000000000, 49.99999999999998579 ) ) ;
#1317 = CARTESIAN_POINT ( 'NONE',  ( -133.6084294554693770, -80.28749220512220575, 37.65825502569592942 ) ) ;
#1318 = LINE ( 'NONE', #12252, #18375 ) ;
#1319 = VERTEX_POINT ( 'NONE', #4241 ) ;
#1320 = VECTOR ( 'NONE', #18741, 1000.000000000000000 ) ;
#1321 = DIRECTION ( 'NONE',  ( 0.000000000000000000, 1.000000000000000000, 0.000000000000000000 ) ) ;
#1322 = DIRECTION ( 'NONE',  ( -0.6692498792541753394, -0.7430374143461900838, 0.000000000000000000 ) ) ;
#1323 = VERTEX_POINT ( 'NONE', #7411 ) ;
#1324 = AXIS2_PLACEMENT_3D ( 'NONE', #8681, #14918, #2449 ) ;
#1325 = ORIENTED_EDGE ( 'NONE', *, *, #10747, .T. ) ;
#1326 = CARTESIAN_POINT ( 'NONE',  ( 0.000000000000000000, 164.0736214083062805, 60.00000000000000000 ) ) ;
#1327 = ORIENTED_EDGE ( 'NONE', *, *, #11278, .T. ) ;
#1328 = EDGE_CURVE ( 'NONE', #2667, #5218, #13434, .T. ) ;
#1329 = DIRECTION ( 'NONE',  ( 0.000000000000000000, 0.000000000000000000, 1.000000000000000000 ) ) ;
#1330 = LINE ( 'NONE', #18727, #3389 ) ;
#1331 = ORIENTED_EDGE ( 'NONE', *, *, #4320, .F. ) ;
#1332 = CARTESIAN_POINT ( 'NONE',  ( 96.32595581636887516, -115.9457815549181277, 10.03375122140240627 ) ) ;
#1333 = CARTESIAN_POINT ( 'NONE',  ( -51.23821591265114961, -28.63313560863453944, 248.9926560891072143 ) ) ;
#1334 = AXIS2_PLACEMENT_3D ( 'NONE', #17984, #8559, #2430 ) ;
#1335 = CIRCLE ( 'NONE', #15384, 150.0000000000000284 ) ;
#1336 = CARTESIAN_POINT ( 'NONE',  ( -137.6995083356076464, -24.48653385596119847, -14.37849102350654817 ) ) ;
#1337 = CARTESIAN_POINT ( 'NONE',  ( -61.70726652483826058, -12.28122767885825084, 132.4711112102474146 ) ) ;
#1338 =( NAMED_UNIT ( * ) SI_UNIT ( $, .STERADIAN. ) SOLID_ANGLE_UNIT ( ) );
#1339 = ADVANCED_FACE ( 'NONE', ( #11901, #13646, #18364, #1378, #7216, #13540 ), #6094, .T. ) ;
#1340 = CYLINDRICAL_SURFACE ( 'NONE', #18052, 3.224098631618460331 ) ;
#1341 = DIRECTION ( 'NONE',  ( 0.6427876096865458022, -0.7660444431189726844, 0.000000000000000000 ) ) ;
#1342 = CARTESIAN_POINT ( 'NONE',  ( -5.485913980968087245, 1.678175111358129801, 283.5832628385307999 ) ) ;
#1343 = CARTESIAN_POINT ( 'NONE',  ( 82.57283217324942370, -125.2267376009776285, 34.78646775464058294 ) ) ;
#1344 = ORIENTED_EDGE ( 'NONE', *, *, #17094, .T. ) ;
#1345 = AXIS2_PLACEMENT_3D ( 'NONE', #10974, #13736, #19980 ) ;
#1346 = CARTESIAN_POINT ( 'NONE',  ( -12.14957802882752524, -59.51724408343569905, 293.5832628385307999 ) ) ;
#1347 = DIRECTION ( 'NONE',  ( -0.000000000000000000, -0.000000000000000000, 1.000000000000000000 ) ) ;
#1348 = ORIENTED_EDGE ( 'NONE', *, *, #401, .F. ) ;
#1349 = AXIS2_PLACEMENT_3D ( 'NONE', #5968, #6073, #13726 ) ;
#1350 = ORIENTED_EDGE ( 'NONE', *, *, #2790, .T. ) ;
#1351 = DIRECTION ( 'NONE',  ( 1.000000000000000000, 0.000000000000000000, 0.000000000000000000 ) ) ;
#1352 = AXIS2_PLACEMENT_3D ( 'NONE', #11177, #3211, #9451 ) ;
#1353 = VERTEX_POINT ( 'NONE', #2819 ) ;
#1354 = EDGE_CURVE ( 'NONE', #8307, #6254, #12104, .T. ) ;
#1355 = FACE_BOUND ( 'NONE', #9430, .T. ) ;
#1356 = VERTEX_POINT ( 'NONE', #12005 ) ;
#1357 = CARTESIAN_POINT ( 'NONE',  ( 0.000000000000000000, 0.000000000000000000, 4.999999999999948486 ) ) ;
#1358 = CYLINDRICAL_SURFACE ( 'NONE', #9937, 7.500000000000020428 ) ;
#1359 = CARTESIAN_POINT ( 'NONE',  ( 0.000000000000000000, 0.000000000000000000, 283.5832628385307999 ) ) ;
#1360 = LINE ( 'NONE', #4427, #16225 ) ;
#1361 = CYLINDRICAL_SURFACE ( 'NONE', #13666, 3.224098631618460331 ) ;
#1362 = ORIENTED_EDGE ( 'NONE', *, *, #17062, .T. ) ;
#1363 = LINE ( 'NONE', #10556, #11446 ) ;
#1364 = FACE_OUTER_BOUND ( 'NONE', #20043, .T. ) ;
#1365 = EDGE_CURVE ( 'NONE', #11921, #6772, #2714, .T. ) ;
#1366 = CARTESIAN_POINT ( 'NONE',  ( 134.4035813917316489, -75.29664220372379191, 5.426846287067242258 ) ) ;
#1367 = DIRECTION ( 'NONE',  ( 0.000000000000000000, 0.000000000000000000, 1.000000000000000000 ) ) ;
#1368 = FACE_OUTER_BOUND ( 'NONE', #18180, .T. ) ;
#1369 = CARTESIAN_POINT ( 'NONE',  ( -134.5311723999394928, -74.37598470588039845, 33.61633749600996879 ) ) ;
#1370 = ORIENTED_EDGE ( 'NONE', *, *, #10229, .T. ) ;
#1371 = EDGE_CURVE ( 'NONE', #7864, #8547, #19790, .T. ) ;
#1372 = FACE_OUTER_BOUND ( 'NONE', #9523, .T. ) ;
#1373 = CIRCLE ( 'NONE', #19355, 60.74260934110282051 ) ;
#1374 = VERTEX_POINT ( 'NONE', #5994 ) ;
#1375 = VERTEX_POINT ( 'NONE', #4555 ) ;
#1376 = ADVANCED_FACE ( 'NONE', ( #7608 ), #8843, .F. ) ;
#1377 = ORIENTED_EDGE ( 'NONE', *, *, #8468, .F. ) ;
#1378 = FACE_BOUND ( 'NONE', #16104, .T. ) ;
#1379 = CIRCLE ( 'NONE', #3344, 79.75827554147308263 ) ;
#1380 = CARTESIAN_POINT ( 'NONE',  ( 118.3534152657848608, 114.7431683447366595, 60.00000000000000000 ) ) ;
#1381 = ORIENTED_EDGE ( 'NONE', *, *, #135, .F. ) ;
#1382 = VECTOR ( 'NONE', #13012, 1000.000000000000000 ) ;
#1383 = CARTESIAN_POINT ( 'NONE',  ( -0.2993243175131910516, 5.729042578294293975, 283.5832628385307999 ) ) ;
#1384 = CARTESIAN_POINT ( 'NONE',  ( 113.5802308907675666, 8.308367629983374414, 14.88498244535465709 ) ) ;
#1385 = ORIENTED_EDGE ( 'NONE', *, *, #16744, .T. ) ;
#1386 = CARTESIAN_POINT ( 'NONE',  ( -83.06695335563966864, 111.5579632196524500, -17.35780129461798538 ) ) ;
#1387 = CARTESIAN_POINT ( 'NONE',  ( 60.00000000000000711, 6.284666409917639535E-13, -115.0000000000000000 ) ) ;
#1388 = CYLINDRICAL_SURFACE ( 'NONE', #4552, 32.50000000000000000 ) ;
#1389 = EDGE_CURVE ( 'NONE', #19700, #2129, #4445, .T. ) ;
#1390 = CIRCLE ( 'NONE', #8571, 150.0000000000000284 ) ;
#1391 = CARTESIAN_POINT ( 'NONE',  ( 0.5612050131688013366, 4.355613924421562366, 9.000000000000003553 ) ) ;
#1392 = CARTESIAN_POINT ( 'NONE',  ( 41.02350267428969488, 44.79940644582669051, 293.5832628385307999 ) ) ;
#1393 = EDGE_CURVE ( 'NONE', #12098, #7664, #16631, .T. ) ;
#1394 = CARTESIAN_POINT ( 'NONE',  ( 131.2732777714562076, -90.85536658133244714, 40.00000000000000000 ) ) ;
#1395 = DIRECTION ( 'NONE',  ( -1.000000000000000000, 0.000000000000000000, 0.000000000000000000 ) ) ;
#1396 = ORIENTED_EDGE ( 'NONE', *, *, #13762, .T. ) ;
#1397 = EDGE_LOOP ( 'NONE', ( #6065, #18802, #5539, #5111 ) ) ;
#1398 = CARTESIAN_POINT ( 'NONE',  ( -42.50000000000000000, 5.204748896376250896E-15, -120.0000000000000142 ) ) ;
#1399 = AXIS2_PLACEMENT_3D ( 'NONE', #2989, #13922, #17212 ) ;
#1400 = AXIS2_PLACEMENT_3D ( 'NONE', #17477, #9487, #3450 ) ;
#1401 = VERTEX_POINT ( 'NONE', #10676 ) ;
#1402 = EDGE_LOOP ( 'NONE', ( #11155, #2446, #12157, #14344 ) ) ;
#1403 = DIRECTION ( 'NONE',  ( -0.000000000000000000, -0.000000000000000000, 1.000000000000000000 ) ) ;
#1404 = ADVANCED_FACE ( 'NONE', ( #16931 ), #2617, .F. ) ;
#1405 = ORIENTED_EDGE ( 'NONE', *, *, #14893, .F. ) ;
#1406 = CARTESIAN_POINT ( 'NONE',  ( 67.08601213326539892, 40.32479851956840378, 248.9926560891072143 ) ) ;
#1407 = CIRCLE ( 'NONE', #20017, 77.50000000000000000 ) ;
#1408 = CARTESIAN_POINT ( 'NONE',  ( -0.4239815141812765531, 0.2650276884262135479, 283.5832628385307999 ) ) ;
#1409 = CARTESIAN_POINT ( 'NONE',  ( -39.84224160888947353, -67.36461649554524911, 132.4711112102474146 ) ) ;
#1410 = CARTESIAN_POINT ( 'NONE',  ( 0.000000000000000000, 0.000000000000000000, 283.5832628385307999 ) ) ;
#1411 = ORIENTED_EDGE ( 'NONE', *, *, #10835, .F. ) ;
#1412 = LINE ( 'NONE', #12242, #6082 ) ;
#1413 = FACE_OUTER_BOUND ( 'NONE', #530, .T. ) ;
#1414 = VERTEX_POINT ( 'NONE', #10470 ) ;
#1415 =( BOUNDED_CURVE ( )  B_SPLINE_CURVE ( 3, ( #2820, #16725, #13854, #16632 ),
 .UNSPECIFIED., .F., .F. ) 
 B_SPLINE_CURVE_WITH_KNOTS ( ( 4, 4 ),
 ( 3.141592653589793116, 4.712388980384689674 ),
 .UNSPECIFIED. ) 
 CURVE ( )  GEOMETRIC_REPRESENTATION_ITEM ( )  RATIONAL_B_SPLINE_CURVE ( ( 1.000000000000000000, 0.8047378541243649375, 0.8047378541243649375, 1.000000000000000000 ) ) 
 REPRESENTATION_ITEM ( '' )  );
#1416 = CARTESIAN_POINT ( 'NONE',  ( -12.14957802882752524, -59.51724408343569905, 293.5832628385307999 ) ) ;
#1418 = CIRCLE ( 'NONE', #15461, 150.0000000000000284 ) ;
#1417 = CARTESIAN_POINT ( 'NONE',  ( 0.000000000000000000, 0.000000000000000000, 132.4711112102474146 ) ) ;
#1419 = VECTOR ( 'NONE', #19266, 999.9999999999998863 ) ;
#1420 = EDGE_CURVE ( 'NONE', #1786, #11921, #13852, .T. ) ;
#1421 = LINE ( 'NONE', #4278, #2460 ) ;
#1422 = CARTESIAN_POINT ( 'NONE',  ( 67.36461649554532016, -39.84224160888924615, 248.9926560891072143 ) ) ;
#1423 = AXIS2_PLACEMENT_3D ( 'NONE', #17058, #18904, #3048 ) ;
#1424 = CARTESIAN_POINT ( 'NONE',  ( -131.2498835542439508, -90.93927553429134036, 39.99999999999999289 ) ) ;
#1425 = CARTESIAN_POINT ( 'NONE',  ( -83.58825350932089293, 112.3093012886738933, 27.97855158061992498 ) ) ;
#1426 = EDGE_CURVE ( 'NONE', #4586, #15527, #20094, .T. ) ;
#1427 = EDGE_LOOP ( 'NONE', ( #19804, #8340, #5647, #20218 ) ) ;
#1428 = FACE_OUTER_BOUND ( 'NONE', #19658, .T. ) ;
#1429 = DIRECTION ( 'NONE',  ( 1.000000000000000000, 0.000000000000000000, 0.000000000000000000 ) ) ;
#1430 = ORIENTED_EDGE ( 'NONE', *, *, #6776, .F. ) ;
#1431 = ORIENTED_EDGE ( 'NONE', *, *, #13655, .F. ) ;
#1432 = LINE ( 'NONE', #7662, #6172 ) ;
#1433 = ORIENTED_EDGE ( 'NONE', *, *, #6415, .F. ) ;
#1434 = LINE ( 'NONE', #7665, #9081 ) ;
#1435 = DIRECTION ( 'NONE',  ( 0.000000000000000000, 0.000000000000000000, 1.000000000000000000 ) ) ;
#1436 = ORIENTED_EDGE ( 'NONE', *, *, #6559, .F. ) ;
#1437 = AXIS2_PLACEMENT_3D ( 'NONE', #7897, #130, #6381 ) ;
#1438 = CARTESIAN_POINT ( 'NONE',  ( 97.49999999995861799, -115.4778303846967020, 10.07710907076146256 ) ) ;
#1439 = FACE_OUTER_BOUND ( 'NONE', #17566, .T. ) ;
#1440 = VECTOR ( 'NONE', #14395, 1000.000000000000000 ) ;
#1441 = CARTESIAN_POINT ( 'NONE',  ( -140.2567302494690011, -18.79374017066554359, -19.65745941995908552 ) ) ;
#1442 = CARTESIAN_POINT ( 'NONE',  ( 11.73417718768049056, 61.81362617575106810, 248.9926560891072143 ) ) ;
#1443 = ORIENTED_EDGE ( 'NONE', *, *, #1629, .F. ) ;
#1444 = FACE_OUTER_BOUND ( 'NONE', #9113, .T. ) ;
#1445 = DIRECTION ( 'NONE',  ( -0.000000000000000000, -0.000000000000000000, -1.000000000000000000 ) ) ;
#1446 = CARTESIAN_POINT ( 'NONE',  ( 12.78021302872850562, -77.21438937758507848, 248.9926560891072143 ) ) ;
#1447 = CARTESIAN_POINT ( 'NONE',  ( 97.99247315425165539, -133.3057953413762391, 33.10491197978900857 ) ) ;
#1448 = ORIENTED_EDGE ( 'NONE', *, *, #3247, .F. ) ;
#1449 = LINE ( 'NONE', #5852, #9070 ) ;
#1450 = DIRECTION ( 'NONE',  ( -0.000000000000000000, -1.000000000000000000, -0.000000000000000000 ) ) ;
#1451 = VERTEX_POINT ( 'NONE', #1166 ) ;
#1452 = AXIS2_PLACEMENT_3D ( 'NONE', #11252, #11149, #5031 ) ;
#1453 = ORIENTED_EDGE ( 'NONE', *, *, #13485, .F. ) ;
#1454 = APPLICATION_PROTOCOL_DEFINITION ( 'draft international standard', 'automotive_design', 1998, #15871 ) ;
#1455 = VECTOR ( 'NONE', #8627, 1000.000000000000000 ) ;
#1456 = ORIENTED_EDGE ( 'NONE', *, *, #12727, .T. ) ;
#1457 = CARTESIAN_POINT ( 'NONE',  ( -97.63534213009850760, -133.7771032679720236, 8.343656291551381443 ) ) ;
#1458 = CARTESIAN_POINT ( 'NONE',  ( 31.77187437101505907, 51.77076963420835654, 283.5832628385307999 ) ) ;
#1459 = ORIENTED_EDGE ( 'NONE', *, *, #17351, .F. ) ;
#1460 = CARTESIAN_POINT ( 'NONE',  ( 12.14914984460760827, 59.51523122377248853, 283.5832628385307999 ) ) ;
#1461 = CARTESIAN_POINT ( 'NONE',  ( -14.69786621328394283, 22.52834316112731017, 39.88498244535555415 ) ) ;
#1462 = CARTESIAN_POINT ( 'NONE',  ( -100.8144812491492672, -129.3825068912777567, 37.43847687706861649 ) ) ;
#1463 = VECTOR ( 'NONE', #9695, 1000.000000000000000 ) ;
#1464 = DIRECTION ( 'NONE',  ( 1.000000000000000000, 0.000000000000000000, 0.000000000000000000 ) ) ;
#1465 = CARTESIAN_POINT ( 'NONE',  ( 0.000000000000000000, 0.000000000000000000, 293.5832628385307999 ) ) ;
#1466 = DIRECTION ( 'NONE',  ( -0.000000000000000000, -0.000000000000000000, 1.000000000000000000 ) ) ;
#1467 = CARTESIAN_POINT ( 'NONE',  ( -132.5536774537036990, -70.21235394457674772, -2.536984270055062662 ) ) ;
#1468 = CARTESIAN_POINT ( 'NONE',  ( 126.7459963399620335, -80.26907437896497299, -1.007255671578283662 ) ) ;
#1469 = CARTESIAN_POINT ( 'NONE',  ( -2.629250726500700353, -60.68567895461850981, 283.5832628385307999 ) ) ;
#1470 = CARTESIAN_POINT ( 'NONE',  ( 4.196299268919053915, 3.911853314815666671, 293.5832628385307999 ) ) ;
#1471 = CARTESIAN_POINT ( 'NONE',  ( -134.4035813917338373, -75.29664220372494299, 34.57315371292968109 ) ) ;
#1472 = EDGE_CURVE ( 'NONE', #8799, #13849, #8940, .T. ) ;
#1473 = ORIENTED_EDGE ( 'NONE', *, *, #16771, .T. ) ;
#1474 = PRODUCT ( 'MOTOR', 'MOTOR', '', ( #6680 ) ) ;
#1475 = LINE ( 'NONE', #18773, #12818 ) ;
#1476 = AXIS2_PLACEMENT_3D ( 'NONE', #15111, #17998, #7440 ) ;
#1477 = VERTEX_POINT ( 'NONE', #16724 ) ;
#1478 = VECTOR ( 'NONE', #14562, 1000.000000000000000 ) ;
#1479 = VERTEX_POINT ( 'NONE', #967 ) ;
#1480 = ADVANCED_FACE ( 'NONE', ( #4143 ), #7310, .F. ) ;
#1481 = ORIENTED_EDGE ( 'NONE', *, *, #16634, .T. ) ;
#1482 = EDGE_CURVE ( 'NONE', #15468, #2215, #15287, .T. ) ;
#1483 = CARTESIAN_POINT ( 'NONE',  ( -141.8038962792965378, -18.44224925282824756, -9.618166193112273277 ) ) ;
#1484 = EDGE_CURVE ( 'NONE', #9791, #19232, #143, .T. ) ;
#1485 = DIRECTION ( 'NONE',  ( 0.1736481776669241694, 0.9848077530122092416, -0.000000000000000000 ) ) ;
#1486 = LINE ( 'NONE', #10885, #16280 ) ;
#1487 = VERTEX_POINT ( 'NONE', #17141 ) ;
#1489 = CARTESIAN_POINT ( 'NONE',  ( -139.8142396999973585, -2.751439320878092509, -13.33333333333314918 ) ) ;
#1488 = VECTOR ( 'NONE', #19524, 1000.000000000000000 ) ;
#1490 = CARTESIAN_POINT ( 'NONE',  ( 8.939227532413712041, -60.08331549348429235, 283.5832628385307999 ) ) ;
#1491 = ORIENTED_EDGE ( 'NONE', *, *, #4117, .F. ) ;
#1492 = CARTESIAN_POINT ( 'NONE',  ( -102.5322778132580623, 84.80111478313182261, -29.20113617578324394 ) ) ;
#1493 = CARTESIAN_POINT ( 'NONE',  ( -58.69016442926522359, 0.8220851292433277724, 132.4711112102474146 ) ) ;
#1494 = DIRECTION ( 'NONE',  ( 6.982962677686266711E-15, -0.000000000000000000, 1.000000000000000000 ) ) ;
#1495 = LINE ( 'NONE', #17151, #9162 ) ;
#1496 = CARTESIAN_POINT ( 'NONE',  ( 18.28567271940513450, -57.92709869106715814, 283.5832628385307999 ) ) ;
#1497 = ADVANCED_FACE ( 'NONE', ( #11088 ), #6603, .T. ) ;
#1498 = CARTESIAN_POINT ( 'NONE',  ( 133.2542153457914367, -68.87904111072916180, 40.95291676807742220 ) ) ;
#1499 = DIRECTION ( 'NONE',  ( 0.7660444431189771253, 0.6427876096865404731, 0.000000000000000000 ) ) ;
#1500 = VECTOR ( 'NONE', #13438, 1000.000000000000000 ) ;
#1501 = VERTEX_POINT ( 'NONE', #15497 ) ;
#1502 = EDGE_LOOP ( 'NONE', ( #6929, #6599, #13042, #17266 ) ) ;
#1503 = ORIENTED_EDGE ( 'NONE', *, *, #5665, .F. ) ;
#1504 = ORIENTED_EDGE ( 'NONE', *, *, #5179, .T. ) ;
#1505 = CARTESIAN_POINT ( 'NONE',  ( 5.729042578294149202, 0.2993243175132214717, 283.5832628385307999 ) ) ;
#1506 = ORIENTED_EDGE ( 'NONE', *, *, #8714, .T. ) ;
#1507 = DIRECTION ( 'NONE',  ( -0.9781142164131910732, 0.2080686897406944236, 0.000000000000000000 ) ) ;
#1508 = EDGE_CURVE ( 'NONE', #13730, #17780, #4871, .T. ) ;
#1509 = EDGE_CURVE ( 'NONE', #4476, #12253, #6504, .T. ) ;
#1510 = DIRECTION ( 'NONE',  ( 0.000000000000000000, 0.000000000000000000, 1.000000000000000000 ) ) ;
#1511 = DIRECTION ( 'NONE',  ( -1.000000000000000000, 0.000000000000000000, 0.000000000000000000 ) ) ;
#1512 = ORIENTED_EDGE ( 'NONE', *, *, #899, .F. ) ;
#1513 = LINE ( 'NONE', #10810, #17528 ) ;
#1514 = CARTESIAN_POINT ( 'NONE',  ( 0.000000000000000000, 7.794228634059941818, 4.500000000000007994 ) ) ;
#1515 = AXIS2_PLACEMENT_3D ( 'NONE', #7804, #13076, #3208 ) ;
#1516 = ORIENTED_EDGE ( 'NONE', *, *, #8040, .T. ) ;
#1517 = AXIS2_PLACEMENT_3D ( 'NONE', #15686, #15576, #15255 ) ;
#1518 = PRODUCT_DEFINITION_CONTEXT ( 'detailed design', #14040, 'design' ) ;
#1519 = LINE ( 'NONE', #7852, #19488 ) ;
#1520 = FACE_OUTER_BOUND ( 'NONE', #4411, .T. ) ;
#1521 = CARTESIAN_POINT ( 'NONE',  ( 4.581103194070519358, -3.453261854573403067, 293.5832628385307999 ) ) ;
#1522 = VECTOR ( 'NONE', #10585, 1000.000000000000000 ) ;
#1523 = EDGE_CURVE ( 'NONE', #3549, #1972, #14271, .T. ) ;
#1524 = CARTESIAN_POINT ( 'NONE',  ( 17.50000000000001776, 2.143131898507868643E-15, 60.00000000000000000 ) ) ;
#1525 = CARTESIAN_POINT ( 'NONE',  ( -77.73583826812294717, 116.4358402608469731, 18.59053902802946112 ) ) ;
#1526 = ORIENTED_EDGE ( 'NONE', *, *, #1659, .T. ) ;
#1527 = CARTESIAN_POINT ( 'NONE',  ( 0.000000000000000000, 0.000000000000000000, 132.4711112102474146 ) ) ;
#1528 = ORIENTED_EDGE ( 'NONE', *, *, #8607, .T. ) ;
#1529 = AXIS2_PLACEMENT_3D ( 'NONE', #19924, #15537, #18818 ) ;
#1530 = ORIENTED_EDGE ( 'NONE', *, *, #4656, .F. ) ;
#1531 = CARTESIAN_POINT ( 'NONE',  ( -22.81000261549328911, 58.63718168490508020, 132.4711112102474146 ) ) ;
#1532 = CIRCLE ( 'NONE', #13602, 127.4413876050234649 ) ;
#1533 = ORIENTED_EDGE ( 'NONE', *, *, #12349, .T. ) ;
#1534 = EDGE_CURVE ( 'NONE', #4193, #12149, #3718, .T. ) ;
#1535 = EDGE_CURVE ( 'NONE', #11442, #8543, #15600, .T. ) ;
#1536 = CARTESIAN_POINT ( 'NONE',  ( -119.9704660726194447, 76.33180017260909267, -33.75105398353568376 ) ) ;
#1537 = VECTOR ( 'NONE', #15562, 1000.000000000000114 ) ;
#1538 = CARTESIAN_POINT ( 'NONE',  ( 37.09555676056997697, -45.48770046196272432, 110.7293897666001214 ) ) ;
#1539 = ORIENTED_EDGE ( 'NONE', *, *, #14292, .F. ) ;
#1540 = CARTESIAN_POINT ( 'NONE',  ( 98.15405843558612276, -133.0926928925950108, 6.371349999020706534 ) ) ;
#1541 = LINE ( 'NONE', #7974, #8014 ) ;
#1542 = ADVANCED_FACE ( 'NONE', ( #15808 ), #19086, .T. ) ;
#1543 = EDGE_CURVE ( 'NONE', #6114, #17930, #5067, .T. ) ;
#1544 = CARTESIAN_POINT ( 'NONE',  ( -148.9554720520392834, -17.67108784863415494, 49.99999999999999289 ) ) ;
#1545 = FACE_BOUND ( 'NONE', #8932, .T. ) ;
#1546 = ORIENTED_EDGE ( 'NONE', *, *, #2756, .F. ) ;
#1547 = FACE_OUTER_BOUND ( 'NONE', #3646, .T. ) ;
#1548 = DIRECTION ( 'NONE',  ( 1.000000000000000000, 0.000000000000000000, 0.000000000000000000 ) ) ;
#1549 = FACE_OUTER_BOUND ( 'NONE', #20139, .T. ) ;
#1550 = CARTESIAN_POINT ( 'NONE',  ( 101.9588377999792925, -127.6928792353687641, 38.34752785143055576 ) ) ;
#1551 = VERTEX_POINT ( 'NONE', #1792 ) ;
#1552 = AXIS2_PLACEMENT_3D ( 'NONE', #4912, #17489, #14204 ) ;
#1553 = CARTESIAN_POINT ( 'NONE',  ( -81.99056186900673993, -84.64042930812179577, 14.88498244535602488 ) ) ;
#1554 = DIRECTION ( 'NONE',  ( -0.3747554100459959403, -0.9271237148521535021, 0.000000000000000000 ) ) ;
#1555 = EDGE_LOOP ( 'NONE', ( #4358, #10280, #171, #524 ) ) ;
#1556 = ORIENTED_EDGE ( 'NONE', *, *, #10730, .F. ) ;
#1557 = ORIENTED_EDGE ( 'NONE', *, *, #18119, .T. ) ;
#1558 = DIRECTION ( 'NONE',  ( 0.000000000000000000, 0.000000000000000000, 1.000000000000000000 ) ) ;
#1559 = ORIENTED_EDGE ( 'NONE', *, *, #10321, .T. ) ;
#1560 = CARTESIAN_POINT ( 'NONE',  ( -32.62092819947992695, -51.24245927909985454, 293.5832628385307999 ) ) ;
#1561 = CARTESIAN_POINT ( 'NONE',  ( 79.05640494598115708, -127.4758205975433043, 49.99999999999999289 ) ) ;
#1562 = VERTEX_POINT ( 'NONE', #10884 ) ;
#1563 = PLANE ( 'NONE',  #16759 ) ;
#1564 = CARTESIAN_POINT ( 'NONE',  ( -29.99999999999887379, 285.0000000000000568, 4.999999999999158007 ) ) ;
#1565 = DIRECTION ( 'NONE',  ( 0.03505990758545895342, 0.9993852124581886764, 0.000000000000000000 ) ) ;
#1566 = VECTOR ( 'NONE', #7488, 1000.000000000000000 ) ;
#1567 = AXIS2_PLACEMENT_3D ( 'NONE', #1346, #18647, #7680 ) ;
#1568 = CARTESIAN_POINT ( 'NONE',  ( -99.15486248080428311, -131.7338018236256119, 35.52123310008073531 ) ) ;
#1569 = CARTESIAN_POINT ( 'NONE',  ( 12.28122767885846223, -61.70726652483821084, 132.4711112102474146 ) ) ;
#1570 = DIRECTION ( 'NONE',  ( 0.000000000000000000, 0.000000000000000000, -1.000000000000000000 ) ) ;
#1571 = DIRECTION ( 'NONE',  ( -0.000000000000000000, -0.000000000000000000, 1.000000000000000000 ) ) ;
#1572 = FACE_BOUND ( 'NONE', #10667, .T. ) ;
#1573 = LINE ( 'NONE', #17231, #70 ) ;
#1574 = LINE ( 'NONE', #9031, #2977 ) ;
#1575 = CARTESIAN_POINT ( 'NONE',  ( 30.05702882063027914, 50.41613078340812848, 110.9660488491356887 ) ) ;
#1576 = CARTESIAN_POINT ( 'NONE',  ( -130.0531662534324653, -74.83651286710070849, 39.27204895968475284 ) ) ;
#1577 = ORIENTED_EDGE ( 'NONE', *, *, #4142, .T. ) ;
#1578 = CARTESIAN_POINT ( 'NONE',  ( 97.50000000000001421, -133.9542832461881119, 10.00000000000000178 ) ) ;
#1579 = AXIS2_PLACEMENT_3D ( 'NONE', #1380, #7217, #12522 ) ;
#1580 = ORIENTED_EDGE ( 'NONE', *, *, #1259, .F. ) ;
#1581 = ORIENTED_EDGE ( 'NONE', *, *, #6806, .T. ) ;
#1582 = ORIENTED_EDGE ( 'NONE', *, *, #17137, .F. ) ;
#1583 = CARTESIAN_POINT ( 'NONE',  ( -144.0486063771584213, -15.28376807748173682, -3.119549641089998548 ) ) ;
#1584 = EDGE_CURVE ( 'NONE', #11084, #12677, #9359, .T. ) ;
#1585 = DIRECTION ( 'NONE',  ( 0.3420201433256694901, -0.9396926207859082059, 0.000000000000000000 ) ) ;
#1586 = DIRECTION ( 'NONE',  ( -0.9848077530122066880, -0.1736481776669374644, 0.000000000000000000 ) ) ;
#1587 = ORIENTED_EDGE ( 'NONE', *, *, #12086, .F. ) ;
#1588 = VECTOR ( 'NONE', #17796, 1000.000000000000000 ) ;
#1589 = CARTESIAN_POINT ( 'NONE',  ( -67.50000000000000000, -2.085703952312275003E-13, -100.0000000000000000 ) ) ;
#1590 = DIRECTION ( 'NONE',  ( 1.000000000000000000, -0.000000000000000000, -0.000000000000000000 ) ) ;
#1591 = AXIS2_PLACEMENT_3D ( 'NONE', #18205, #10727, #2968 ) ;
#1592 = AXIS2_PLACEMENT_3D ( 'NONE', #14625, #6663, #9920 ) ;
#1593 = ORIENTED_EDGE ( 'NONE', *, *, #649, .T. ) ;
#1594 = CARTESIAN_POINT ( 'NONE',  ( -80.58504095603038309, 114.1753459096158565, -13.99979793087933366 ) ) ;
#1595 = AXIS2_PLACEMENT_3D ( 'NONE', #2928, #14068, #6309 ) ;
#1596 = PLANE ( 'NONE',  #15083 ) ;
#1597 = DIRECTION ( 'NONE',  ( 1.000000000000000000, 0.000000000000000000, 0.000000000000000000 ) ) ;
#1598 = DIRECTION ( 'NONE',  ( 0.000000000000000000, 0.000000000000000000, -1.000000000000000000 ) ) ;
#1599 = DIRECTION ( 'NONE',  ( 0.3088643371590125142, -0.9511061040868803440, 0.000000000000000000 ) ) ;
#1600 = ORIENTED_EDGE ( 'NONE', *, *, #3125, .F. ) ;
#1601 = EDGE_CURVE ( 'NONE', #18954, #8910, #6203, .T. ) ;
#1602 = DIRECTION ( 'NONE',  ( 0.6427876096865430267, -0.7660444431189749048, 0.000000000000000000 ) ) ;
#1603 = CARTESIAN_POINT ( 'NONE',  ( -122.8001410695374602, -86.14014948502067170, -10.00000000000000178 ) ) ;
#1604 = EDGE_LOOP ( 'NONE', ( #11796, #250, #431, #18706 ) ) ;
#1605 = ADVANCED_FACE ( 'NONE', ( #9257 ), #52, .T. ) ;
#1606 = ORIENTED_EDGE ( 'NONE', *, *, #16687, .F. ) ;
#1607 = ORIENTED_EDGE ( 'NONE', *, *, #17136, .F. ) ;
#1608 = VECTOR ( 'NONE', #12347, 1000.000000000000000 ) ;
#1609 = CIRCLE ( 'NONE', #9455, 60.74260934110282051 ) ;
#1610 = ORIENTED_EDGE ( 'NONE', *, *, #6423, .F. ) ;
#1611 = CARTESIAN_POINT ( 'NONE',  ( 107.5000000000000284, -199.9999999999999716, 0.000000000000000000 ) ) ;
#1612 = AXIS2_PLACEMENT_3D ( 'NONE', #19576, #2494, #2400 ) ;
#1613 = ORIENTED_EDGE ( 'NONE', *, *, #3498, .F. ) ;
#1614 = CARTESIAN_POINT ( 'NONE',  ( 7.950000000000000178, -10.39230484541326582, 0.000000000000000000 ) ) ;
#1615 = EDGE_CURVE ( 'NONE', #7758, #11142, #3427, .T. ) ;
#1616 = CARTESIAN_POINT ( 'NONE',  ( -97.49999999999995737, -133.9542832461881687, 30.48494313689572977 ) ) ;
#1617 = DIRECTION ( 'NONE',  ( 1.000000000000000000, 0.000000000000000000, -0.000000000000000000 ) ) ;
#1618 = DIRECTION ( 'NONE',  ( -0.8660254037844363761, -0.5000000000000039968, 0.000000000000000000 ) ) ;
#1619 = DIRECTION ( 'NONE',  ( -0.000000000000000000, -0.000000000000000000, 1.000000000000000000 ) ) ;
#1620 = ORIENTED_EDGE ( 'NONE', *, *, #8861, .F. ) ;
#1621 = CARTESIAN_POINT ( 'NONE',  ( 53.40063514825076396, 28.94886449118923721, 283.5832628385307999 ) ) ;
#1622 = LINE ( 'NONE', #17175, #2585 ) ;
#1623 = ORIENTED_EDGE ( 'NONE', *, *, #5733, .T. ) ;
#1624 = CARTESIAN_POINT ( 'NONE',  ( -79.97569708437522706, 124.9326907832373053, -21.45256608093599127 ) ) ;
#1625 = DIRECTION ( 'NONE',  ( -0.8830229359480271656, -0.4693298356057563625, 0.000000000000000000 ) ) ;
#1626 = AXIS2_PLACEMENT_3D ( 'NONE', #11664, #11570, #6779 ) ;
#1627 = VECTOR ( 'NONE', #18990, 1000.000000000000000 ) ;
#1628 = LINE ( 'NONE', #6639, #7663 ) ;
#1629 = EDGE_CURVE ( 'NONE', #19246, #9958, #15910, .T. ) ;
#1630 = CARTESIAN_POINT ( 'NONE',  ( -75.71267875615025389, -86.11264925328200093, 14.88498244535597870 ) ) ;
#1631 = ADVANCED_FACE ( 'NONE', ( #12521 ), #18783, .F. ) ;
#1632 = CARTESIAN_POINT ( 'NONE',  ( 85.53020504959901871, -140.9188050298377846, 60.00000000000000000 ) ) ;
#1633 = DIRECTION ( 'NONE',  ( 6.982962677686266711E-15, -0.000000000000000000, 1.000000000000000000 ) ) ;
#1634 = VERTEX_POINT ( 'NONE', #10986 ) ;
#1635 = ADVANCED_FACE ( 'NONE', ( #17245 ), #13312, .F. ) ;
#1636 = DIRECTION ( 'NONE',  ( -0.1736481776669206722, -0.9848077530122096857, 0.000000000000000000 ) ) ;
#1637 = EDGE_LOOP ( 'NONE', ( #6576, #3214, #91, #19853 ) ) ;
#1638 = ORIENTED_EDGE ( 'NONE', *, *, #989, .T. ) ;
#1639 = CARTESIAN_POINT ( 'NONE',  ( 0.000000000000000000, 0.000000000000000000, 248.9926560891072143 ) ) ;
#1640 = ORIENTED_EDGE ( 'NONE', *, *, #7107, .T. ) ;
#1641 = DIRECTION ( 'NONE',  ( -0.000000000000000000, -0.000000000000000000, -1.000000000000000000 ) ) ;
#1642 = EDGE_CURVE ( 'NONE', #3721, #2271, #16487, .T. ) ;
#1643 = ADVANCED_BREP_SHAPE_REPRESENTATION ( '', ( #14854, #18639 ), #12 ) ;
#1644 = ORIENTED_EDGE ( 'NONE', *, *, #9146, .T. ) ;
#1645 = CARTESIAN_POINT ( 'NONE',  ( 97.50000000000000000, -133.9542832461674777, 9.627394560795542233 ) ) ;
#1646 = DIRECTION ( 'NONE',  ( 1.000000000000000000, 0.000000000000000000, 0.000000000000000000 ) ) ;
#1647 = LINE ( 'NONE', #6357, #17013 ) ;
#1648 = DIRECTION ( 'NONE',  ( -6.982962677686266711E-15, 0.000000000000000000, -1.000000000000000000 ) ) ;
#1649 = ORIENTED_EDGE ( 'NONE', *, *, #15735, .T. ) ;
#1650 = DIRECTION ( 'NONE',  ( 0.000000000000000000, 0.000000000000000000, -1.000000000000000000 ) ) ;
#1651 = CARTESIAN_POINT ( 'NONE',  ( -145.8139347833763111, 34.97575719557632823, -12.90182706766672105 ) ) ;
#1652 = CARTESIAN_POINT ( 'NONE',  ( 0.000000000000000000, 0.000000000000000000, 293.5832628385307999 ) ) ;
#1653 = EDGE_CURVE ( 'NONE', #9691, #10395, #16414, .T. ) ;
#1654 = DIRECTION ( 'NONE',  ( 6.982962677686266711E-15, -0.000000000000000000, 1.000000000000000000 ) ) ;
#1655 = AXIS2_PLACEMENT_3D ( 'NONE', #6154, #13497, #5743 ) ;
#1656 = CARTESIAN_POINT ( 'NONE',  ( 95.64785785032829324, -115.7351073148938099, 34.14437575866686103 ) ) ;
#1657 = EDGE_LOOP ( 'NONE', ( #11287, #15226, #11669 ) ) ;
#1658 = EDGE_CURVE ( 'NONE', #13976, #15168, #5364, .T. ) ;
#1659 = EDGE_CURVE ( 'NONE', #7429, #1375, #8429, .T. ) ;
#1660 = CARTESIAN_POINT ( 'NONE',  ( 56.50329132715945235, -22.30005961346246579, 293.5832628385307999 ) ) ;
#1661 = CARTESIAN_POINT ( 'NONE',  ( -70.66508887821294138, 132.3119617713222738, 12.27828551785295019 ) ) ;
#1662 = ORIENTED_EDGE ( 'NONE', *, *, #11670, .T. ) ;
#1663 = ORIENTED_EDGE ( 'NONE', *, *, #7409, .T. ) ;
#1664 = EDGE_LOOP ( 'NONE', ( #700, #9748, #5019, #14210 ) ) ;
#1665 = EDGE_LOOP ( 'NONE', ( #14610, #8264, #5272, #7279 ) ) ;
#1666 = CARTESIAN_POINT ( 'NONE',  ( -99.75239863728833711, -130.9022835076664819, 3.666872587888030832 ) ) ;
#1667 = FACE_BOUND ( 'NONE', #10726, .T. ) ;
#1668 = ORIENTED_EDGE ( 'NONE', *, *, #10953, .T. ) ;
#1669 = VECTOR ( 'NONE', #12429, 1000.000000000000000 ) ;
#1670 = CYLINDRICAL_SURFACE ( 'NONE', #7935, 7.500000000000002665 ) ;
#1671 = CARTESIAN_POINT ( 'NONE',  ( -2.300765332208190905, -116.0870680293436408, 39.88498244535547599 ) ) ;
#1672 = CARTESIAN_POINT ( 'NONE',  ( -60.00000000000000000, -2.094888803305880013E-13, -115.0000000000000000 ) ) ;
#1673 = CARTESIAN_POINT ( 'NONE',  ( -96.05623471149394277, -115.3294058443304522, 35.20016690035954809 ) ) ;
#1674 = LINE ( 'NONE', #5228, #9676 ) ;
#1675 = CARTESIAN_POINT ( 'NONE',  ( -100.7812499999999716, -111.0996833858562809, -10.00000000000000178 ) ) ;
#1676 = CARTESIAN_POINT ( 'NONE',  ( 27.50000000000001776, 3.367778697655222096E-15, 43.88498244535526993 ) ) ;
#1677 = EDGE_CURVE ( 'NONE', #17774, #1634, #12213, .T. ) ;
#1678 = CARTESIAN_POINT ( 'NONE',  ( -60.00000000000000000, -2.094888803305880013E-13, -105.0000000000000142 ) ) ;
#1679 = DIRECTION ( 'NONE',  ( 1.000000000000000000, 0.000000000000000000, 0.000000000000000000 ) ) ;
#1680 = CARTESIAN_POINT ( 'NONE',  ( -127.3242258594542875, -79.35722205890316161, 40.89109837179960039 ) ) ;
#1681 = VERTEX_POINT ( 'NONE', #19287 ) ;
#1682 = AXIS2_PLACEMENT_3D ( 'NONE', #2629, #13551, #19903 ) ;
#1683 = LINE ( 'NONE', #7814, #9557 ) ;
#1684 = VECTOR ( 'NONE', #15696, 1000.000000000000000 ) ;
#1685 = EDGE_CURVE ( 'NONE', #16315, #16184, #6704, .T. ) ;
#1686 = ORIENTED_EDGE ( 'NONE', *, *, #17649, .F. ) ;
#1687 = EDGE_LOOP ( 'NONE', ( #10284, #14904, #13754, #3544 ) ) ;
#1688 = EDGE_LOOP ( 'NONE', ( #7188, #16034, #5863 ) ) ;
#1689 = CARTESIAN_POINT ( 'NONE',  ( 26.04958516073451236, 47.87779272208936021, 248.9926560891072143 ) ) ;
#1690 = CARTESIAN_POINT ( 'NONE',  ( -152.4599531637108498, -36.50981547337168109, 60.00000000000000000 ) ) ;
#1691 = CARTESIAN_POINT ( 'NONE',  ( 77.50000000000000000, 0.000000000000000000, -115.0000000000000000 ) ) ;
#1692 = ORIENTED_EDGE ( 'NONE', *, *, #9501, .T. ) ;
#1693 = DIRECTION ( 'NONE',  ( 1.000000000000000000, 0.000000000000000000, 0.000000000000000000 ) ) ;
#1694 = DIRECTION ( 'NONE',  ( 6.982962677686266711E-15, -0.000000000000000000, 1.000000000000000000 ) ) ;
#1695 = DIRECTION ( 'NONE',  ( 1.000000000000000000, 0.000000000000000000, -6.977185866873308817E-15 ) ) ;
#1696 = CARTESIAN_POINT ( 'NONE',  ( -19.79297637435836421, 18.57624240429761642, 14.88498244535559145 ) ) ;
#1697 = DIRECTION ( 'NONE',  ( 1.000000000000000000, 0.000000000000000000, 0.000000000000000000 ) ) ;
#1698 = ORIENTED_EDGE ( 'NONE', *, *, #16107, .F. ) ;
#1699 = CARTESIAN_POINT ( 'NONE',  ( 132.3557670345053907, -70.70247614045412377, 35.47327301125541510 ) ) ;
#1700 = CARTESIAN_POINT ( 'NONE',  ( 132.6188226329610984, -85.30892464212138293, 39.27175784426802352 ) ) ;
#1701 = EDGE_LOOP ( 'NONE', ( #3307, #2684, #15104 ) ) ;
#1702 = VERTEX_POINT ( 'NONE', #16317 ) ;
#1703 = EDGE_LOOP ( 'NONE', ( #9563, #5259, #2824, #1057 ) ) ;
#1704 = ORIENTED_EDGE ( 'NONE', *, *, #3413, .T. ) ;
#1705 = CARTESIAN_POINT ( 'NONE',  ( -23.22718332831480481, -56.12853591711337486, 293.5832628385307999 ) ) ;
#1706 = VECTOR ( 'NONE', #463, 1000.000000000000000 ) ;
#1707 = ORIENTED_EDGE ( 'NONE', *, *, #14056, .F. ) ;
#1708 = CYLINDRICAL_SURFACE ( 'NONE', #3475, 3.224098631618460331 ) ;
#1709 = DIRECTION ( 'NONE',  ( -0.7660444431189835646, 0.6427876096865328126, 0.000000000000000000 ) ) ;
#1710 = DIRECTION ( 'NONE',  ( -0.5300553768524376430, -0.8479630283625698706, 0.000000000000000000 ) ) ;
#1711 = CARTESIAN_POINT ( 'NONE',  ( 0.000000000000000000, 164.0736214083062805, 49.99999999999999289 ) ) ;
#1712 = ORIENTED_EDGE ( 'NONE', *, *, #11528, .F. ) ;
#1713 = CARTESIAN_POINT ( 'NONE',  ( -55.16472960512350454, 30.25670013172272732, 248.9926560891072143 ) ) ;
#1714 = LINE ( 'NONE', #18815, #19892 ) ;
#1715 = ORIENTED_EDGE ( 'NONE', *, *, #18056, .T. ) ;
#1716 = CYLINDRICAL_SURFACE ( 'NONE', #20141, 9.999999999999994671 ) ;
#1717 = LINE ( 'NONE', #20130, #18249 ) ;
#1718 = DIRECTION ( 'NONE',  ( 1.000000000000000000, 0.000000000000000000, 0.000000000000000000 ) ) ;
#1719 = VECTOR ( 'NONE', #11438, 999.9999999999998863 ) ;
#1720 = DIRECTION ( 'NONE',  ( -0.000000000000000000, -0.000000000000000000, 1.000000000000000000 ) ) ;
#1721 = CARTESIAN_POINT ( 'NONE',  ( 56.84754764479240663, -154.7316448359447634, 49.99999999999999289 ) ) ;
#1722 = CARTESIAN_POINT ( 'NONE',  ( -75.72815543956944850, 117.7508209023505970, -2.114875207142446367 ) ) ;
#1723 = ORIENTED_EDGE ( 'NONE', *, *, #1272, .F. ) ;
#1724 = EDGE_CURVE ( 'NONE', #13875, #15125, #846, .T. ) ;
#1725 = PLANE ( 'NONE',  #116 ) ;
#1726 = ORIENTED_EDGE ( 'NONE', *, *, #13356, .F. ) ;
#1727 = AXIS2_PLACEMENT_3D ( 'NONE', #16670, #1633, #18506 ) ;
#1728 = ORIENTED_EDGE ( 'NONE', *, *, #16609, .T. ) ;
#1729 = DIRECTION ( 'NONE',  ( -0.000000000000000000, -0.000000000000000000, 1.000000000000000000 ) ) ;
#1730 = EDGE_LOOP ( 'NONE', ( #1704, #11388 ) ) ;
#1731 = CYLINDRICAL_SURFACE ( 'NONE', #17927, 62.91752772691707207 ) ;
#1732 = EDGE_CURVE ( 'NONE', #17702, #7714, #16013, .T. ) ;
#1733 = DIRECTION ( 'NONE',  ( 1.000000000000000000, 0.000000000000000000, -6.977185866873309606E-15 ) ) ;
#1734 = CIRCLE ( 'NONE', #18728, 60.74260934110282051 ) ;
#1735 = ORIENTED_EDGE ( 'NONE', *, *, #7341, .T. ) ;
#1736 = AXIS2_PLACEMENT_3D ( 'NONE', #12948, #13138, #19497 ) ;
#1737 = ADVANCED_FACE ( 'NONE', ( #3921 ), #14862, .T. ) ;
#1738 = SURFACE_STYLE_USAGE ( .BOTH. , #16167 ) ;
#1739 = CARTESIAN_POINT ( 'NONE',  ( 0.000000000000000000, 0.000000000000000000, 293.5832628385307999 ) ) ;
#1740 = EDGE_CURVE ( 'NONE', #6676, #16987, #17142, .T. ) ;
#1741 = FACE_OUTER_BOUND ( 'NONE', #834, .T. ) ;
#1742 = AXIS2_PLACEMENT_3D ( 'NONE', #15415, #10698, #16954 ) ;
#1743 = DIRECTION ( 'NONE',  ( 6.982962677686266711E-15, -0.000000000000000000, 1.000000000000000000 ) ) ;
#1744 = LINE ( 'NONE', #17711, #4727 ) ;
#1745 = VERTEX_POINT ( 'NONE', #562 ) ;
#1746 = DIRECTION ( 'NONE',  ( 1.000000000000000000, 0.000000000000000000, 0.000000000000000000 ) ) ;
#1747 = AXIS2_PLACEMENT_3D ( 'NONE', #1538, #15551, #12055 ) ;
#1748 = CARTESIAN_POINT ( 'NONE',  ( -6.191009641800430785, -26.42934155884822900, 14.88498244535549375 ) ) ;
#1749 = CARTESIAN_POINT ( 'NONE',  ( -56.12662799072088404, 23.22641211976270625, 283.5832628385307999 ) ) ;
#1750 = CARTESIAN_POINT ( 'NONE',  ( -110.0000000000000142, 285.0000000000000568, 5.000000000000000888 ) ) ;
#1751 = ORIENTED_EDGE ( 'NONE', *, *, #989, .F. ) ;
#1752 = EDGE_CURVE ( 'NONE', #19819, #16530, #16152, .T. ) ;
#1753 = DIRECTION ( 'NONE',  ( -0.000000000000000000, -0.000000000000000000, 1.000000000000000000 ) ) ;
#1754 = CARTESIAN_POINT ( 'NONE',  ( -96.99644974731859293, 114.4709739857757285, 42.93971707143836625 ) ) ;
#1755 = VECTOR ( 'NONE', #18931, 1000.000000000000000 ) ;
#1756 = ORIENTED_EDGE ( 'NONE', *, *, #272, .T. ) ;
#1757 = ORIENTED_EDGE ( 'NONE', *, *, #7286, .F. ) ;
#1758 = ORIENTED_EDGE ( 'NONE', *, *, #4080, .F. ) ;
#1759 = VECTOR ( 'NONE', #16906, 1000.000000000000000 ) ;
#1760 = ORIENTED_EDGE ( 'NONE', *, *, #17363, .F. ) ;
#1761 = CARTESIAN_POINT ( 'NONE',  ( -97.77474281578803073, -133.5937942518638124, 7.660502963261819787 ) ) ;
#1762 = CARTESIAN_POINT ( 'NONE',  ( -111.7004912049619492, 100.1461745756109138, 44.99999999999997868 ) ) ;
#1763 = MECHANICAL_DESIGN_GEOMETRIC_PRESENTATION_REPRESENTATION (  '', ( #18100 ), #5359 ) ;
#1764 = ORIENTED_EDGE ( 'NONE', *, *, #10036, .F. ) ;
#1765 = EDGE_CURVE ( 'NONE', #16453, #5784, #19740, .T. ) ;
#1766 = LINE ( 'NONE', #6282, #14801 ) ;
#1767 = LINE ( 'NONE', #18967, #10903 ) ;
#1768 = CARTESIAN_POINT ( 'NONE',  ( 134.6604885881914129, -66.08112487034739502, 35.71876651910825728 ) ) ;
#1769 = EDGE_CURVE ( 'NONE', #7001, #4216, #2900, .T. ) ;
#1770 = PRODUCT_DEFINITION ( 'UNKNOWN', '', #13424, #9290 ) ;
#1771 = CARTESIAN_POINT ( 'NONE',  ( -98.78819505924192867, -132.2357222602873605, 34.91288608638632951 ) ) ;
#1772 = LINE ( 'NONE', #17336, #18832 ) ;
#1773 = CARTESIAN_POINT ( 'NONE',  ( 25.99419088092191643, -73.82206860051539365, 132.4711112102474146 ) ) ;
#1774 = CARTESIAN_POINT ( 'NONE',  ( 0.000000000000000000, 0.000000000000000000, 0.000000000000000000 ) ) ;
#1775 = PLANE ( 'NONE',  #19420 ) ;
#1776 = CARTESIAN_POINT ( 'NONE',  ( 36.99514631729018532, -48.17959877923561862, 293.5832628385307999 ) ) ;
#1777 = CIRCLE ( 'NONE', #8629, 3.224098631618458999 ) ;
#1778 = DIRECTION ( 'NONE',  ( 0.000000000000000000, 0.000000000000000000, 1.000000000000000000 ) ) ;
#1779 = LINE ( 'NONE', #3514, #8208 ) ;
#1780 = CARTESIAN_POINT ( 'NONE',  ( -131.4291603288542944, -72.40192386451013817, 37.44902174672004946 ) ) ;
#1781 = ORIENTED_EDGE ( 'NONE', *, *, #844, .F. ) ;
#1782 = ADVANCED_FACE ( 'NONE', ( #12080 ), #4425, .T. ) ;
#1783 = LINE ( 'NONE', #17548, #15777 ) ;
#1784 = AXIS2_PLACEMENT_3D ( 'NONE', #15184, #13748, #19894 ) ;
#1785 = EDGE_LOOP ( 'NONE', ( #14903, #9584 ) ) ;
#1786 = VERTEX_POINT ( 'NONE', #9126 ) ;
#1787 = VERTEX_POINT ( 'NONE', #2594 ) ;
#1788 = EDGE_CURVE ( 'NONE', #12640, #10824, #16909, .T. ) ;
#1789 = EDGE_CURVE ( 'NONE', #2612, #7835, #16170, .T. ) ;
#1790 = VECTOR ( 'NONE', #8875, 1000.000000000000114 ) ;
#1791 = ADVANCED_FACE ( 'NONE', ( #5662 ), #9021, .F. ) ;
#1792 = CARTESIAN_POINT ( 'NONE',  ( 32.64570716507540737, -53.78543575132140830, 132.4711112102474146 ) ) ;
#1793 = DIRECTION ( 'NONE',  ( -0.1736481776669207000, -0.9848077530122097967, 0.000000000000000000 ) ) ;
#1794 = DIRECTION ( 'NONE',  ( 0.9848077530122091305, -0.1736481776669241417, 0.000000000000000000 ) ) ;
#1795 = EDGE_CURVE ( 'NONE', #11036, #13843, #13283, .T. ) ;
#1796 = LINE ( 'NONE', #12732, #8766 ) ;
#1797 = DIRECTION ( 'NONE',  ( 0.5000000000000038858, 0.8660254037844362651, -3.503961184244744203E-15 ) ) ;
#1798 = CARTESIAN_POINT ( 'NONE',  ( 0.000000000000000000, 0.000000000000000000, 49.99999999999999289 ) ) ;
#1799 = FACE_BOUND ( 'NONE', #7536, .T. ) ;
#1800 = VECTOR ( 'NONE', #17404, 1000.000000000000114 ) ;
#1801 = DIRECTION ( 'NONE',  ( 6.982962677686266711E-15, -0.000000000000000000, 1.000000000000000000 ) ) ;
#1802 = ORIENTED_EDGE ( 'NONE', *, *, #17084, .T. ) ;
#1803 = CARTESIAN_POINT ( 'NONE',  ( 130.5346569920086779, -73.99347627470881150, 38.71596122396615414 ) ) ;
#1804 = CIRCLE ( 'NONE', #13210, 60.74260934110282051 ) ;
#1805 = CARTESIAN_POINT ( 'NONE',  ( 134.4445132543468446, -75.00751837915895237, 34.30968946414332521 ) ) ;
#1806 = EDGE_LOOP ( 'NONE', ( #13482, #12155, #3837, #11415 ) ) ;
#1807 = VERTEX_POINT ( 'NONE', #16606 ) ;
#1808 = ORIENTED_EDGE ( 'NONE', *, *, #7146, .T. ) ;
#1809 = ORIENTED_EDGE ( 'NONE', *, *, #3158, .F. ) ;
#1810 = LINE ( 'NONE', #8042, #15122 ) ;
#1811 = PRODUCT ( 'Part3^MAS-341', 'Part3^MAS-341', '', ( #8091 ) ) ;
#1812 = ORIENTED_EDGE ( 'NONE', *, *, #15557, .T. ) ;
#1813 = LINE ( 'NONE', #4685, #1854 ) ;
#1814 = AXIS2_PLACEMENT_3D ( 'NONE', #14717, #19236, #2052 ) ;
#1815 = DIRECTION ( 'NONE',  ( -0.5300553768524346454, -0.8479630283625717579, 0.000000000000000000 ) ) ;
#1816 = LINE ( 'NONE', #178, #9053 ) ;
#1817 = ORIENTED_EDGE ( 'NONE', *, *, #17387, .F. ) ;
#1818 = DIRECTION ( 'NONE',  ( 1.000000000000000000, -4.650550193362991910E-16, 0.000000000000000000 ) ) ;
#1819 = DIRECTION ( 'NONE',  ( -0.5000000000000009992, 0.8660254037844380415, 0.000000000000000000 ) ) ;
#1820 = ORIENTED_EDGE ( 'NONE', *, *, #18588, .T. ) ;
#1821 = DIRECTION ( 'NONE',  ( 0.000000000000000000, 0.000000000000000000, -1.000000000000000000 ) ) ;
#1822 = CARTESIAN_POINT ( 'NONE',  ( -156.4179374840092862, -52.02840013024096066, 49.99999999999999289 ) ) ;
#1823 = DIRECTION ( 'NONE',  ( 0.000000000000000000, 0.000000000000000000, -1.000000000000000000 ) ) ;
#1824 = AXIS2_PLACEMENT_3D ( 'NONE', #9990, #3945, #13342 ) ;
#1825 = FACE_OUTER_BOUND ( 'NONE', #5481, .T. ) ;
#1826 = FACE_OUTER_BOUND ( 'NONE', #7645, .T. ) ;
#1827 = CARTESIAN_POINT ( 'NONE',  ( 0.000000000000000000, 0.000000000000000000, 49.99999999999999289 ) ) ;
#1828 = CIRCLE ( 'NONE', #15542, 7.500000000000007105 ) ;
#1829 = CARTESIAN_POINT ( 'NONE',  ( -134.8030718230775449, -47.09494809331346232, 39.99999999999999289 ) ) ;
#1830 = ORIENTED_EDGE ( 'NONE', *, *, #7477, .T. ) ;
#1831 = CARTESIAN_POINT ( 'NONE',  ( 49.67518383744835120, -60.47951622432767493, 110.7293897666001214 ) ) ;
#1832 = ORIENTED_EDGE ( 'NONE', *, *, #3155, .F. ) ;
#1833 = ORIENTED_EDGE ( 'NONE', *, *, #8359, .T. ) ;
#1834 = LINE ( 'NONE', #17082, #18907 ) ;
#1835 = ORIENTED_EDGE ( 'NONE', *, *, #6218, .T. ) ;
#1836 = AXIS2_PLACEMENT_3D ( 'NONE', #1169, #4245, #7414 ) ;
#1837 = DIRECTION ( 'NONE',  ( -0.7660444431189835646, 0.6427876096865328126, 0.000000000000000000 ) ) ;
#1838 = CARTESIAN_POINT ( 'NONE',  ( 37.93579148621461883, 68.46530598706809201, 132.4711112102474146 ) ) ;
#1839 = ORIENTED_EDGE ( 'NONE', *, *, #16386, .F. ) ;
#1840 = FILL_AREA_STYLE_COLOUR ( '', #11290 ) ;
#1841 = CARTESIAN_POINT ( 'NONE',  ( -9.381844291199351815, 57.94128254008192158, 112.0427633081291816 ) ) ;
#1842 = ADVANCED_FACE ( 'NONE', ( #5765 ), #1252, .T. ) ;
#1843 = LINE ( 'NONE', #8280, #16385 ) ;
#1844 = AXIS2_PLACEMENT_3D ( 'NONE', #15301, #1293, #1499 ) ;
#1845 = CARTESIAN_POINT ( 'NONE',  ( 0.8220851292435327196, 62.91215678473957240, 248.9926560891072143 ) ) ;
#1846 = LINE ( 'NONE', #16072, #18111 ) ;
#1847 = VERTEX_POINT ( 'NONE', #13622 ) ;
#1848 = FACE_OUTER_BOUND ( 'NONE', #17236, .T. ) ;
#1849 = CARTESIAN_POINT ( 'NONE',  ( 0.000000000000000000, 0.000000000000000000, 83.57543755549745867 ) ) ;
#1850 = EDGE_CURVE ( 'NONE', #9217, #15200, #9187, .T. ) ;
#1851 = CARTESIAN_POINT ( 'NONE',  ( -60.00000000000000000, -2.094888803305880013E-13, -105.0000000000000142 ) ) ;
#1852 = DIRECTION ( 'NONE',  ( 0.000000000000000000, 0.000000000000000000, 1.000000000000000000 ) ) ;
#1853 = ORIENTED_EDGE ( 'NONE', *, *, #2497, .F. ) ;
#1854 = VECTOR ( 'NONE', #18702, 1000.000000000000114 ) ;
#1855 = EDGE_CURVE ( 'NONE', #858, #9602, #7389, .T. ) ;
#1856 = PLANE ( 'NONE',  #9087 ) ;
#1857 = CARTESIAN_POINT ( 'NONE',  ( -90.95160660477870351, 119.2832880936750399, 40.18161886156921270 ) ) ;
#1858 = ORIENTED_EDGE ( 'NONE', *, *, #14026, .T. ) ;
#1859 = ORIENTED_EDGE ( 'NONE', *, *, #13152, .T. ) ;
#1860 = EDGE_CURVE ( 'NONE', #11048, #19503, #12189, .T. ) ;
#1862 = VERTEX_POINT ( 'NONE', #4019 ) ;
#1861 = AXIS2_PLACEMENT_3D ( 'NONE', #16348, #17885, #10103 ) ;
#1863 = ORIENTED_EDGE ( 'NONE', *, *, #18363, .F. ) ;
#1864 = LINE ( 'NONE', #325, #3263 ) ;
#1865 = CARTESIAN_POINT ( 'NONE',  ( 0.000000000000000000, 0.000000000000000000, 293.5832628385307999 ) ) ;
#1866 = VERTEX_POINT ( 'NONE', #8919 ) ;
#1867 = CARTESIAN_POINT ( 'NONE',  ( -189.9999999999988916, 275.0000000000000000, 5.000000000000268230 ) ) ;
#1868 = FACE_BOUND ( 'NONE', #4582, .T. ) ;
#1869 = CARTESIAN_POINT ( 'NONE',  ( 122.8001410695374744, -86.14014948502065749, 49.99999999999999289 ) ) ;
#1870 = EDGE_CURVE ( 'NONE', #8891, #15066, #11880, .T. ) ;
#1871 = CARTESIAN_POINT ( 'NONE',  ( -93.27226090021295590, -117.4765369300808828, -8.336715671529505656 ) ) ;
#1872 = FACE_OUTER_BOUND ( 'NONE', #3737, .T. ) ;
#1873 = CYLINDRICAL_SURFACE ( 'NONE', #16470, 15.91767397667354089 ) ;
#1874 = VECTOR ( 'NONE', #18951, 1000.000000000000000 ) ;
#1875 = DIRECTION ( 'NONE',  ( 1.000000000000000000, 0.000000000000000000, 0.000000000000000000 ) ) ;
#1876 = DIRECTION ( 'NONE',  ( 1.000000000000000000, 0.000000000000000000, 0.000000000000000000 ) ) ;
#1877 = FACE_OUTER_BOUND ( 'NONE', #6342, .T. ) ;
#1878 = CARTESIAN_POINT ( 'NONE',  ( -122.8001410695374886, -86.14014948502064328, 50.00000000000000000 ) ) ;
#1879 = ORIENTED_EDGE ( 'NONE', *, *, #168, .T. ) ;
#1880 = EDGE_CURVE ( 'NONE', #10402, #19514, #946, .T. ) ;
#1881 = CARTESIAN_POINT ( 'NONE',  ( -138.9607784057693323, 13.84518047783050321, -14.65874628096230836 ) ) ;
#1882 = ADVANCED_FACE ( 'NONE', ( #5866 ), #7198, .F. ) ;
#1883 = EDGE_CURVE ( 'NONE', #17498, #9484, #13516, .T. ) ;
#1884 = ORIENTED_EDGE ( 'NONE', *, *, #12889, .F. ) ;
#1885 = APPLICATION_CONTEXT ( 'automotive_design' ) ;
#1886 = AXIS2_PLACEMENT_3D ( 'NONE', #9686, #1923, #16038 ) ;
#1887 = VERTEX_POINT ( 'NONE', #4317 ) ;
#1888 = CIRCLE ( 'NONE', #17570, 15.91767397667354089 ) ;
#1889 = AXIS2_PLACEMENT_3D ( 'NONE', #8232, #4882, #12736 ) ;
#1890 = EDGE_LOOP ( 'NONE', ( #916, #3438, #11512, #2174 ) ) ;
#1891 = EDGE_CURVE ( 'NONE', #1401, #4820, #9815, .T. ) ;
#1892 = CARTESIAN_POINT ( 'NONE',  ( -11.00103590902911499, -57.65577537092155325, 248.9926560891072143 ) ) ;
#1893 = CARTESIAN_POINT ( 'NONE',  ( -62.91752772691707207, 8.736373289420574370E-15, 83.57543755549745867 ) ) ;
#1894 = CARTESIAN_POINT ( 'NONE',  ( -14.39940464655760799, -76.92888220842476699, 132.4711112102474146 ) ) ;
#1895 = EDGE_LOOP ( 'NONE', ( #421, #9874, #17551 ) ) ;
#1896 = DIRECTION ( 'NONE',  ( -0.000000000000000000, -0.000000000000000000, 1.000000000000000000 ) ) ;
#1897 = LINE ( 'NONE', #11196, #7566 ) ;
#1898 = CARTESIAN_POINT ( 'NONE',  ( -81.99056186900673993, -84.64042930812179577, 14.88498244535602488 ) ) ;
#1899 = CARTESIAN_POINT ( 'NONE',  ( -59.30716253403183202, 13.12726406102060217, 283.5832628385307999 ) ) ;
#1900 = DIRECTION ( 'NONE',  ( -0.1736481776669404620, -0.9848077530122062440, 1.229460064647279239E-15 ) ) ;
#1901 = VERTEX_POINT ( 'NONE', #18945 ) ;
#1902 = CIRCLE ( 'NONE', #9740, 3.224098631618460331 ) ;
#1903 = EDGE_CURVE ( 'NONE', #17877, #8041, #1843, .T. ) ;
#1904 = CARTESIAN_POINT ( 'NONE',  ( 133.7753978164260786, -79.32938232249655641, 37.22355218228292273 ) ) ;
#1905 = EDGE_CURVE ( 'NONE', #10931, #8624, #14525, .T. ) ;
#1906 = LINE ( 'NONE', #9776, #5771 ) ;
#1907 = EDGE_CURVE ( 'NONE', #16556, #4476, #3003, .T. ) ;
#1908 = EDGE_LOOP ( 'NONE', ( #144, #18042, #3141, #15618 ) ) ;
#1909 = ADVANCED_FACE ( 'NONE', ( #5227 ), #6562, .T. ) ;
#1910 = ORIENTED_EDGE ( 'NONE', *, *, #6373, .F. ) ;
#1911 = EDGE_LOOP ( 'NONE', ( #19538, #3190 ) ) ;
#1912 = ORIENTED_EDGE ( 'NONE', *, *, #6675, .F. ) ;
#1913 = DIRECTION ( 'NONE',  ( -0.9993852124581887875, 0.03505990758545545621, 0.000000000000000000 ) ) ;
#1914 = ADVANCED_FACE ( 'NONE', ( #6459 ), #9617, .F. ) ;
#1915 = AXIS2_PLACEMENT_3D ( 'NONE', #4817, #9513, #17085 ) ;
#1916 = EDGE_LOOP ( 'NONE', ( #9131, #3969, #19888, #11350 ) ) ;
#1917 = CARTESIAN_POINT ( 'NONE',  ( -110.0000000000000142, 275.0000000000000000, 5.000000000000000888 ) ) ;
#1918 = CIRCLE ( 'NONE', #18576, 3.224098631618463440 ) ;
#1919 = AXIS2_PLACEMENT_3D ( 'NONE', #13938, #13832, #15479 ) ;
#1920 = CARTESIAN_POINT ( 'NONE',  ( 51.24245927909996112, -32.62092819947974220, 293.5832628385307999 ) ) ;
#1921 = VECTOR ( 'NONE', #5432, 1000.000000000000000 ) ;
#1922 = FILL_AREA_STYLE ('',( #15934 ) ) ;
#1923 = DIRECTION ( 'NONE',  ( -0.1736481776669404620, 0.9848077530122062440, 0.000000000000000000 ) ) ;
#1924 = VERTEX_POINT ( 'NONE', #17605 ) ;
#1925 = CARTESIAN_POINT ( 'NONE',  ( 128.2293354902420788, -77.84035270136641316, -8.157851372385163558 ) ) ;
#1926 = LINE ( 'NONE', #17482, #13030 ) ;
#1927 = ORIENTED_EDGE ( 'NONE', *, *, #18850, .F. ) ;
#1928 = CARTESIAN_POINT ( 'NONE',  ( -108.3191475787680957, 90.65673307763522359, -34.99999999999998579 ) ) ;
#1929 = CYLINDRICAL_SURFACE ( 'NONE', #15307, 42.50000000000000000 ) ;
#1930 = CARTESIAN_POINT ( 'NONE',  ( 0.8220851292435327196, 78.26059000578311498, 248.9926560891072143 ) ) ;
#1931 = LINE ( 'NONE', #17282, #6702 ) ;
#1932 = EDGE_CURVE ( 'NONE', #8191, #1945, #2018, .T. ) ;
#1933 = CARTESIAN_POINT ( 'NONE',  ( -2.629322876227788264, -60.68773558783006905, 293.5832628385307999 ) ) ;
#1934 = CARTESIAN_POINT ( 'NONE',  ( 59.58067424803626011, -20.21777810286696564, 132.4711112102474146 ) ) ;
#1935 = LINE ( 'NONE', #14410, #12622 ) ;
#1936 = VECTOR ( 'NONE', #14201, 1000.000000000000000 ) ;
#1937 = AXIS2_PLACEMENT_3D ( 'NONE', #10093, #14596, #6729 ) ;
#1938 = ORIENTED_EDGE ( 'NONE', *, *, #1997, .T. ) ;
#1939 = AXIS2_PLACEMENT_3D ( 'NONE', #17249, #15813, #1693 ) ;
#1940 = CARTESIAN_POINT ( 'NONE',  ( 78.26059000578312919, -0.8220851292427129309, 112.7772637782949516 ) ) ;
#1941 = VERTEX_POINT ( 'NONE', #1953 ) ;
#1942 = EDGE_CURVE ( 'NONE', #3127, #12874, #11451, .T. ) ;
#1943 = VERTEX_POINT ( 'NONE', #19041 ) ;
#1944 = LINE ( 'NONE', #8173, #2255 ) ;
#1945 = VERTEX_POINT ( 'NONE', #17707 ) ;
#1946 = CARTESIAN_POINT ( 'NONE',  ( 1.396592535537252080E-14, 0.000000000000000000, 49.99999999999998579 ) ) ;
#1947 = PLANE ( 'NONE',  #2408 ) ;
#1948 = ORIENTED_EDGE ( 'NONE', *, *, #15789, .F. ) ;
#1949 = LINE ( 'NONE', #14425, #18148 ) ;
#1950 = DIRECTION ( 'NONE',  ( -0.9902903945359624593, -0.1390141521205945918, 0.000000000000000000 ) ) ;
#1951 = CIRCLE ( 'NONE', #16000, 62.91752772691707207 ) ;
#1952 = AXIS2_PLACEMENT_3D ( 'NONE', #3657, #8252, #9890 ) ;
#1953 = CARTESIAN_POINT ( 'NONE',  ( -110.0000000000000142, 285.0000000000000568, 50.00000000000000000 ) ) ;
#1954 = CARTESIAN_POINT ( 'NONE',  ( -54.07248341783231638, 32.16802499836798290, 132.4711112102474146 ) ) ;
#1955 = CARTESIAN_POINT ( 'NONE',  ( 0.000000000000000000, 0.000000000000000000, 50.00000000000000000 ) ) ;
#1956 = DIRECTION ( 'NONE',  ( -6.982962677686266711E-15, 0.000000000000000000, -1.000000000000000000 ) ) ;
#1957 = ORIENTED_EDGE ( 'NONE', *, *, #6019, .T. ) ;
#1958 = DIRECTION ( 'NONE',  ( -0.9781142164131910732, 0.2080686897406944236, 0.000000000000000000 ) ) ;
#1959 = CARTESIAN_POINT ( 'NONE',  ( 67.36461649554529174, -39.84224160888925326, 132.4711112102474146 ) ) ;
#1960 = CARTESIAN_POINT ( 'NONE',  ( 0.000000000000000000, 0.000000000000000000, 283.5832628385307999 ) ) ;
#1961 = DIRECTION ( 'NONE',  ( -0.000000000000000000, -0.000000000000000000, 1.000000000000000000 ) ) ;
#1962 = EDGE_LOOP ( 'NONE', ( #15435, #18285, #9262, #7046 ) ) ;
#1963 = DIRECTION ( 'NONE',  ( 0.000000000000000000, 1.000000000000000000, 0.000000000000000000 ) ) ;
#1964 = CARTESIAN_POINT ( 'NONE',  ( -74.41710797946193168, 130.2395184813107960, 23.29328984172064310 ) ) ;
#1965 = VERTEX_POINT ( 'NONE', #6755 ) ;
#1966 = AXIS2_PLACEMENT_3D ( 'NONE', #4709, #2970, #9200 ) ;
#1967 = VECTOR ( 'NONE', #4023, 1000.000000000000000 ) ;
#1968 = EDGE_CURVE ( 'NONE', #5595, #19503, #9232, .T. ) ;
#1969 = VERTEX_POINT ( 'NONE', #12679 ) ;
#1970 = VERTEX_POINT ( 'NONE', #7975 ) ;
#1971 = PRODUCT_CONTEXT ( 'NONE', #13758, 'mechanical' ) ;
#1972 = VERTEX_POINT ( 'NONE', #2153 ) ;
#1973 = LINE ( 'NONE', #9940, #18862 ) ;
#1974 = ORIENTED_EDGE ( 'NONE', *, *, #19282, .T. ) ;
#1975 = FILL_AREA_STYLE_COLOUR ( '', #18077 ) ;
#1976 = FACE_OUTER_BOUND ( 'NONE', #19531, .T. ) ;
#1977 = CARTESIAN_POINT ( 'NONE',  ( 0.000000000000000000, 0.000000000000000000, 283.5832628385307999 ) ) ;
#1978 = AXIS2_PLACEMENT_3D ( 'NONE', #521, #2355, #13178 ) ;
#1979 = EDGE_CURVE ( 'NONE', #16478, #7342, #8378, .T. ) ;
#1980 = AXIS2_PLACEMENT_3D ( 'NONE', #4506, #9206, #7367 ) ;
#1981 = CARTESIAN_POINT ( 'NONE',  ( -121.1286015293791394, 70.20561501501187252, 38.18765959548887423 ) ) ;
#1982 = LINE ( 'NONE', #19169, #185 ) ;
#1983 = CARTESIAN_POINT ( 'NONE',  ( 51.36153797460909232, -59.06449708980182578, 248.9926560891072143 ) ) ;
#1984 = CARTESIAN_POINT ( 'NONE',  ( -11.54977938102048007, 57.55901709132182731, 132.4711112102474146 ) ) ;
#1985 = FACE_OUTER_BOUND ( 'NONE', #19871, .T. ) ;
#1986 = PLANE ( 'NONE',  #4620 ) ;
#1987 = CARTESIAN_POINT ( 'NONE',  ( -110.0000000000000142, 0.000000000000000000, 39.99999999999997868 ) ) ;
#1988 = EDGE_LOOP ( 'NONE', ( #8084, #8409, #2017, #10586 ) ) ;
#1989 = CARTESIAN_POINT ( 'NONE',  ( 60.00000000000000711, 6.284666409917639535E-13, -105.0000000000000142 ) ) ;
#1990 = EDGE_CURVE ( 'NONE', #13146, #5943, #11144, .T. ) ;
#1991 = ADVANCED_FACE ( 'NONE', ( #1741 ), #3380, .T. ) ;
#1992 = ORIENTED_EDGE ( 'NONE', *, *, #9300, .F. ) ;
#1993 = VECTOR ( 'NONE', #19337, 1000.000000000000227 ) ;
#1994 = VERTEX_POINT ( 'NONE', #11245 ) ;
#1995 = ORIENTED_EDGE ( 'NONE', *, *, #2272, .F. ) ;
#1996 = DIRECTION ( 'NONE',  ( 0.000000000000000000, 0.000000000000000000, -1.000000000000000000 ) ) ;
#1997 = EDGE_CURVE ( 'NONE', #4838, #6246, #3584, .T. ) ;
#1998 = PLANE ( 'NONE',  #3865 ) ;
#1999 = EDGE_CURVE ( 'NONE', #2094, #6828, #14327, .T. ) ;
#2000 = DIRECTION ( 'NONE',  ( 0.000000000000000000, 0.000000000000000000, 1.000000000000000000 ) ) ;
#2001 = EDGE_CURVE ( 'NONE', #10388, #19150, #8181, .T. ) ;
#2002 = CARTESIAN_POINT ( 'NONE',  ( -79.75827554147308263, 9.767571684737763671E-15, 269.6944534026102360 ) ) ;
#2003 = CIRCLE ( 'NONE', #17696, 3.224098631618460331 ) ;
#2004 = CARTESIAN_POINT ( 'NONE',  ( 32.50000000000000000, 0.000000000000000000, -105.0000000000000142 ) ) ;
#2005 = DIRECTION ( 'NONE',  ( -0.9902903945359630145, -0.1390141521205912334, 0.000000000000000000 ) ) ;
#2006 = CARTESIAN_POINT ( 'NONE',  ( 103.6585128263305222, -125.0478522927852225, 39.23652335784740330 ) ) ;
#2007 = CIRCLE ( 'NONE', #16700, 7.500000000000008882 ) ;
#2008 = DIRECTION ( 'NONE',  ( 0.9781142164131917394, -0.2080686897406911207, 0.000000000000000000 ) ) ;
#2009 = ORIENTED_EDGE ( 'NONE', *, *, #9610, .T. ) ;
#2010 = CARTESIAN_POINT ( 'NONE',  ( 60.08127757648377099, 8.938941455415205795, 283.5832628385307999 ) ) ;
#2011 = VERTEX_POINT ( 'NONE', #606 ) ;
#2012 = EDGE_CURVE ( 'NONE', #1477, #3588, #6661, .T. ) ;
#2013 = VECTOR ( 'NONE', #3418, 1000.000000000000000 ) ;
#2014 = VERTEX_POINT ( 'NONE', #641 ) ;
#2015 = ADVANCED_FACE ( 'NONE', ( #9948 ), #13293, .T. ) ;
#2016 = EDGE_LOOP ( 'NONE', ( #13062, #1109, #19889, #3041 ) ) ;
#2017 = ORIENTED_EDGE ( 'NONE', *, *, #9353, .T. ) ;
#2018 = CIRCLE ( 'NONE', #13747, 7.500000000000002665 ) ;
#2019 = ORIENTED_EDGE ( 'NONE', *, *, #9001, .T. ) ;
#2020 = CARTESIAN_POINT ( 'NONE',  ( 39.37628763770420903, 49.07263256785967087, 293.5832628385307999 ) ) ;
#2021 = PRODUCT_DEFINITION_FORMATION_WITH_SPECIFIED_SOURCE ( 'ANY', '', #18804, .NOT_KNOWN. ) ;
#2022 = LINE ( 'NONE', #8150, #9900 ) ;
#2023 = DIRECTION ( 'NONE',  ( 1.000000000000000000, 0.000000000000000000, -6.977185866873308817E-15 ) ) ;
#2024 = ORIENTED_EDGE ( 'NONE', *, *, #9144, .F. ) ;
#2025 = ADVANCED_FACE ( 'NONE', ( #17933 ), #16199, .F. ) ;
#2026 = DIRECTION ( 'NONE',  ( -1.000000000000000000, 2.775557561562888984E-15, 0.000000000000000000 ) ) ;
#2027 = CARTESIAN_POINT ( 'NONE',  ( 103.2967819461769921, 53.25886146954521649, 39.88498244535472992 ) ) ;
#2028 = ADVANCED_FACE ( 'NONE', ( #16395 ), #4096, .T. ) ;
#2029 = VERTEX_POINT ( 'NONE', #929 ) ;
#2030 = EDGE_CURVE ( 'NONE', #10487, #3058, #19649, .T. ) ;
#2031 = CARTESIAN_POINT ( 'NONE',  ( -53.40063514825077107, -28.94886449118923011, 293.5832628385307999 ) ) ;
#2032 = CARTESIAN_POINT ( 'NONE',  ( 152.4599531637113330, -36.50981547336952104, 60.00000000000000000 ) ) ;
#2033 = DIRECTION ( 'NONE',  ( 1.000000000000000000, 0.000000000000000000, -0.000000000000000000 ) ) ;
#2034 = DIRECTION ( 'NONE',  ( 6.982962677686266711E-15, -0.000000000000000000, 1.000000000000000000 ) ) ;
#2035 = CARTESIAN_POINT ( 'NONE',  ( 152.4599531637113330, -36.50981547336952104, 60.00000000000000000 ) ) ;
#2036 = DIRECTION ( 'NONE',  ( -6.982962677686266711E-15, 0.000000000000000000, -1.000000000000000000 ) ) ;
#2037 = CYLINDRICAL_SURFACE ( 'NONE', #2496, 7.500000000000008882 ) ;
#2038 = ORIENTED_EDGE ( 'NONE', *, *, #15262, .F. ) ;
#2039 = ADVANCED_FACE ( 'NONE', ( #18524 ), #15242, .F. ) ;
#2040 = DIRECTION ( 'NONE',  ( -0.000000000000000000, -0.000000000000000000, 1.000000000000000000 ) ) ;
#2041 = CIRCLE ( 'NONE', #17726, 60.74260934110282051 ) ;
#2042 = ORIENTED_EDGE ( 'NONE', *, *, #19006, .T. ) ;
#2043 = EDGE_LOOP ( 'NONE', ( #19758, #18949 ) ) ;
#2044 = LINE ( 'NONE', #19612, #16763 ) ;
#2045 = ORIENTED_EDGE ( 'NONE', *, *, #3986, .T. ) ;
#2046 = DIRECTION ( 'NONE',  ( 0.000000000000000000, 0.000000000000000000, 1.000000000000000000 ) ) ;
#2047 = LINE ( 'NONE', #8277, #14496 ) ;
#2048 = ORIENTED_EDGE ( 'NONE', *, *, #14538, .F. ) ;
#2049 = ADVANCED_FACE ( 'NONE', ( #13600 ), #19846, .F. ) ;
#2050 = EDGE_CURVE ( 'NONE', #16647, #4108, #4200, .T. ) ;
#2051 = FILL_AREA_STYLE ('',( #1840 ) ) ;
#2052 = DIRECTION ( 'NONE',  ( -1.000000000000000000, 0.000000000000000000, 6.969309079188926949E-15 ) ) ;
#2053 = CARTESIAN_POINT ( 'NONE',  ( -12.16118437606778535, -23.99289710269258080, 14.88498244535553461 ) ) ;
#2055 = CIRCLE ( 'NONE', #9879, 7.500000000000008882 ) ;
#2054 = FACE_OUTER_BOUND ( 'NONE', #10517, .T. ) ;
#2056 = VECTOR ( 'NONE', #6463, 1000.000000000000000 ) ;
#2057 = EDGE_CURVE ( 'NONE', #13334, #14067, #16787, .T. ) ;
#2058 = DIRECTION ( 'NONE',  ( 1.000000000000000000, 0.000000000000000000, 0.000000000000000000 ) ) ;
#2059 = CARTESIAN_POINT ( 'NONE',  ( -18.28503710798546678, 57.92514141135459482, 283.5832628385307999 ) ) ;
#2060 = ORIENTED_EDGE ( 'NONE', *, *, #14600, .T. ) ;
#2061 = CARTESIAN_POINT ( 'NONE',  ( 63.68887634719570912, -147.8252249328912740, 39.99999999999999289 ) ) ;
#2062 = PLANE ( 'NONE',  #7087 ) ;
#2063 = AXIS2_PLACEMENT_3D ( 'NONE', #5235, #6862, #9720 ) ;
#2064 = CARTESIAN_POINT ( 'NONE',  ( 0.000000000000000000, 0.000000000000000000, -39.99999999999999289 ) ) ;
#2065 = FACE_OUTER_BOUND ( 'NONE', #633, .T. ) ;
#2066 = EDGE_LOOP ( 'NONE', ( #20041, #7947, #14391, #7069 ) ) ;
#2067 = LINE ( 'NONE', #4834, #13328 ) ;
#2068 = CARTESIAN_POINT ( 'NONE',  ( -70.79267019417842732, 132.2446714760112059, -3.125962082761043703 ) ) ;
#2069 = ORIENTED_EDGE ( 'NONE', *, *, #9873, .T. ) ;
#2070 = ORIENTED_EDGE ( 'NONE', *, *, #15491, .F. ) ;
#2071 = VERTEX_POINT ( 'NONE', #8804 ) ;
#2072 = ITEM_DEFINED_TRANSFORMATION ( 'NONE', 'NONE', #17666,  #18639 ) ;
#2073 = VECTOR ( 'NONE', #9324, 1000.000000000000114 ) ;
#2074 = VECTOR ( 'NONE', #15472, 999.9999999999998863 ) ;
#2075 = ORIENTED_EDGE ( 'NONE', *, *, #3500, .F. ) ;
#2076 = DIRECTION ( 'NONE',  ( -0.9902903945359624593, -0.1390141521205945918, 0.000000000000000000 ) ) ;
#2077 = LINE ( 'NONE', #11065, #10031 ) ;
#2078 = ORIENTED_EDGE ( 'NONE', *, *, #9346, .T. ) ;
#2079 = VECTOR ( 'NONE', #9482, 1000.000000000000000 ) ;
#2080 = DIRECTION ( 'NONE',  ( -1.000000000000000000, -0.000000000000000000, -0.000000000000000000 ) ) ;
#2081 = CARTESIAN_POINT ( 'NONE',  ( -85.14104117559512019, -123.4951580371804170, -1.036462382361432288 ) ) ;
#2082 = ORIENTED_EDGE ( 'NONE', *, *, #2486, .T. ) ;
#2083 = CARTESIAN_POINT ( 'NONE',  ( -140.0000000000000284, 1.714505518806295230E-14, 23.02775637731986436 ) ) ;
#2084 = SHAPE_REPRESENTATION ( 'Main Body', ( #18639 ), #15396 ) ;
#2085 = DIRECTION ( 'NONE',  ( 0.000000000000000000, 0.000000000000000000, -1.000000000000000000 ) ) ;
#2086 = AXIS2_PLACEMENT_3D ( 'NONE', #790, #13357, #2531 ) ;
#2087 = CARTESIAN_POINT ( 'NONE',  ( -163.5019688434124419, -20.99123081650240863, 39.99999999999999289 ) ) ;
#2088 = DIRECTION ( 'NONE',  ( 0.000000000000000000, 0.000000000000000000, -1.000000000000000000 ) ) ;
#2089 = DIRECTION ( 'NONE',  ( -6.982962677686266711E-15, 0.000000000000000000, -1.000000000000000000 ) ) ;
#2090 = VERTEX_POINT ( 'NONE', #1337 ) ;
#2091 = CARTESIAN_POINT ( 'NONE',  ( -139.1660152614074093, 12.14097363381727668, -14.35026434167516918 ) ) ;
#2092 = AXIS2_PLACEMENT_3D ( 'NONE', #19183, #655, #3920 ) ;
#2093 = COLOUR_RGB ( '', 0.40784314, 0.44705882, 0.49803922) ;
#2094 = VERTEX_POINT ( 'NONE', #13705 ) ;
#2095 = ORIENTED_EDGE ( 'NONE', *, *, #1769, .T. ) ;
#2096 = ORIENTED_EDGE ( 'NONE', *, *, #8530, .T. ) ;
#2097 = DIRECTION ( 'NONE',  ( 0.000000000000000000, 0.000000000000000000, 1.000000000000000000 ) ) ;
#2098 = CARTESIAN_POINT ( 'NONE',  ( -132.4160198941376336, -70.47193775266624982, -2.820813203610496700 ) ) ;
#2099 = CARTESIAN_POINT ( 'NONE',  ( -58.63718168490499494, -22.81000261549348807, 293.5832628385307999 ) ) ;
#2100 = AXIS2_PLACEMENT_3D ( 'NONE', #5154, #16091, #11379 ) ;
#2101 = DIRECTION ( 'NONE',  ( 0.000000000000000000, 0.000000000000000000, 1.000000000000000000 ) ) ;
#2102 = EDGE_CURVE ( 'NONE', #15527, #19079, #4609, .T. ) ;
#2103 = CARTESIAN_POINT ( 'NONE',  ( 0.000000000000000000, 164.0736214083062805, 39.99999999999999289 ) ) ;
#2104 = CARTESIAN_POINT ( 'NONE',  ( 1.289614712049185874, -5.590028426173808462, 283.5832628385307999 ) ) ;
#2105 = CARTESIAN_POINT ( 'NONE',  ( 67.50000000000000000, 6.284666409917639535E-13, -105.0000000000000142 ) ) ;
#2106 = VECTOR ( 'NONE', #11427, 1000.000000000000114 ) ;
#2107 = CARTESIAN_POINT ( 'NONE',  ( 98.50852301078391804, -132.6154683359945352, 34.39645643909215522 ) ) ;
#2108 = CARTESIAN_POINT ( 'NONE',  ( 7.500000000000001776, 60.00000000000000000, -105.0000000000000142 ) ) ;
#2109 = VERTEX_POINT ( 'NONE', #15142 ) ;
#2110 = ORIENTED_EDGE ( 'NONE', *, *, #18540, .T. ) ;
#2111 = ORIENTED_EDGE ( 'NONE', *, *, #17400, .F. ) ;
#2112 = ADVANCED_FACE ( 'NONE', ( #1025 ), #2572, .T. ) ;
#2113 = VERTEX_POINT ( 'NONE', #2877 ) ;
#2114 = ADVANCED_FACE ( 'NONE', ( #10629 ), #7271, .T. ) ;
#2115 = CIRCLE ( 'NONE', #14846, 112.8770930172170353 ) ;
#2116 = EDGE_LOOP ( 'NONE', ( #18057, #19985, #17004, #1580 ) ) ;
#2117 = ADVANCED_FACE ( 'NONE', ( #1125 ), #12060, .F. ) ;
#2118 = DIRECTION ( 'NONE',  ( 0.000000000000000000, 1.000000000000000000, 0.000000000000000000 ) ) ;
#2119 = AXIS2_PLACEMENT_3D ( 'NONE', #18139, #19667, #10551 ) ;
#2120 = ORIENTED_EDGE ( 'NONE', *, *, #18776, .F. ) ;
#2121 = FACE_OUTER_BOUND ( 'NONE', #16081, .T. ) ;
#2122 = CYLINDRICAL_SURFACE ( 'NONE', #8302, 60.74260934110282051 ) ;
#2123 = CARTESIAN_POINT ( 'NONE',  ( 0.000000000000000000, 0.000000000000000000, 269.6944534026102360 ) ) ;
#2124 = EDGE_LOOP ( 'NONE', ( #8641, #17677, #10547, #9555 ) ) ;
#2126 = CIRCLE ( 'NONE', #16820, 10.00000000000000178 ) ;
#2125 = DIRECTION ( 'NONE',  ( 6.982962677686266711E-15, 0.000000000000000000, 1.000000000000000000 ) ) ;
#2127 = CARTESIAN_POINT ( 'NONE',  ( -56.84754764479025368, -154.7316448359455308, 39.99999999999999289 ) ) ;
#2128 = EDGE_CURVE ( 'NONE', #18905, #12093, #8842, .T. ) ;
#2129 = VERTEX_POINT ( 'NONE', #6933 ) ;
#2130 = DIRECTION ( 'NONE',  ( 0.000000000000000000, 0.000000000000000000, 1.000000000000000000 ) ) ;
#2131 = CARTESIAN_POINT ( 'NONE',  ( 0.000000000000000000, 0.000000000000000000, -120.0000000000000142 ) ) ;
#2132 = AXIS2_PLACEMENT_3D ( 'NONE', #2703, #10267, #8358 ) ;
#2133 = CYLINDRICAL_SURFACE ( 'NONE', #18006, 7.500000000000007105 ) ;
#2134 = CARTESIAN_POINT ( 'NONE',  ( 47.56406379474552182, 37.78325588002191893, 283.5832628385307999 ) ) ;
#2135 = DIRECTION ( 'NONE',  ( -1.000000000000000000, 8.881784197001250351E-16, 0.000000000000000000 ) ) ;
#2136 = FACE_OUTER_BOUND ( 'NONE', #8142, .T. ) ;
#2137 = CARTESIAN_POINT ( 'NONE',  ( 93.80830170559224257, -117.0490297264385191, 48.57545654425775439 ) ) ;
#2138 = EDGE_LOOP ( 'NONE', ( #12512, #19684, #12449, #17623, #12034 ) ) ;
#2139 = ADVANCED_FACE ( 'NONE', ( #9996, #6542 ), #12763, .T. ) ;
#2140 = LINE ( 'NONE', #17790, #20045 ) ;
#2141 = ORIENTED_EDGE ( 'NONE', *, *, #4483, .F. ) ;
#2142 = EDGE_CURVE ( 'NONE', #18256, #16743, #5301, .T. ) ;
#2143 = VECTOR ( 'NONE', #3874, 1000.000000000000000 ) ;
#2144 = ORIENTED_EDGE ( 'NONE', *, *, #8858, .F. ) ;
#2145 = EDGE_CURVE ( 'NONE', #6039, #10395, #7534, .T. ) ;
#2146 = DIRECTION ( 'NONE',  ( 1.000000000000000000, 0.000000000000000000, 0.000000000000000000 ) ) ;
#2147 = CONICAL_SURFACE ( 'NONE', #3034, 9.000000000000000000, 1.047197551196600296 ) ;
#2148 = ORIENTED_EDGE ( 'NONE', *, *, #2258, .F. ) ;
#2149 = CARTESIAN_POINT ( 'NONE',  ( 44.43084819159276577, -38.35506425062471436, 110.7293897666001214 ) ) ;
#2150 = CARTESIAN_POINT ( 'NONE',  ( -82.03124999999995737, -125.5821405433014348, 30.72794638160199554 ) ) ;
#2151 = CARTESIAN_POINT ( 'NONE',  ( 0.3570196857253480904, -9.540868182094900618, -1.474731560294321175 ) ) ;
#2152 = DIRECTION ( 'NONE',  ( -1.000000000000000000, 0.000000000000000000, 0.000000000000000000 ) ) ;
#2153 = CARTESIAN_POINT ( 'NONE',  ( 37.93579148621461172, 68.46530598706807780, 248.9926560891072143 ) ) ;
#2154 = EDGE_CURVE ( 'NONE', #18469, #16270, #19417, .T. ) ;
#2155 = PRODUCT_DEFINITION_SHAPE ( 'NONE', 'NONE',  #8137 ) ;
#2156 = CYLINDRICAL_SURFACE ( 'NONE', #1515, 112.8770930172170068 ) ;
#2157 = CARTESIAN_POINT ( 'NONE',  ( 98.17567701213377518, -133.0624052623788316, 6.362069460218656936 ) ) ;
#2158 = VECTOR ( 'NONE', #8073, 1000.000000000000000 ) ;
#2159 = DIRECTION ( 'NONE',  ( 1.000000000000000000, 0.000000000000000000, -6.977185866873308817E-15 ) ) ;
#2160 = LINE ( 'NONE', #14628, #17800 ) ;
#2161 = ORIENTED_EDGE ( 'NONE', *, *, #5553, .T. ) ;
#2162 = DIRECTION ( 'NONE',  ( -0.8479630283625716469, 0.5300553768524345344, 0.000000000000000000 ) ) ;
#2163 = DIRECTION ( 'NONE',  ( 1.000000000000000000, 0.000000000000000000, -6.994638739193269649E-15 ) ) ;
#2164 = CARTESIAN_POINT ( 'NONE',  ( 87.50000000000004263, -133.9542832461881119, 49.99999999999999289 ) ) ;
#2165 = FACE_BOUND ( 'NONE', #2281, .T. ) ;
#2166 = ORIENTED_EDGE ( 'NONE', *, *, #2145, .F. ) ;
#2167 = DIRECTION ( 'NONE',  ( 0.000000000000000000, 0.000000000000000000, 1.000000000000000000 ) ) ;
#2168 = DIRECTION ( 'NONE',  ( -1.000000000000000000, 0.000000000000000000, 0.000000000000000000 ) ) ;
#2169 = EDGE_CURVE ( 'NONE', #3058, #5289, #19323, .T. ) ;
#2170 = VERTEX_POINT ( 'NONE', #15944 ) ;
#2172 = ADVANCED_FACE ( 'NONE', ( #8056 ), #2133, .F. ) ;
#2171 = AXIS2_PLACEMENT_3D ( 'NONE', #7203, #10261, #7102 ) ;
#2173 = VERTEX_POINT ( 'NONE', #6834 ) ;
#2174 = ORIENTED_EDGE ( 'NONE', *, *, #10355, .F. ) ;
#2175 = APPLICATION_PROTOCOL_DEFINITION ( 'draft international standard', 'automotive_design', 1998, #1885 ) ;
#2176 = EDGE_LOOP ( 'NONE', ( #12386, #890, #5115, #11167 ) ) ;
#2177 = ADVANCED_FACE ( 'NONE', ( #16047 ), #13058, .F. ) ;
#2178 = VECTOR ( 'NONE', #8074, 1000.000000000000000 ) ;
#2179 = CARTESIAN_POINT ( 'NONE',  ( -120.3490144071938346, 89.54138470860034715, 43.64576342102566286 ) ) ;
#2180 = ORIENTED_EDGE ( 'NONE', *, *, #5365, .T. ) ;
#2181 = FACE_OUTER_BOUND ( 'NONE', #2915, .T. ) ;
#2182 = DIRECTION ( 'NONE',  ( -0.6427876096865430267, 0.7660444431189749048, 0.000000000000000000 ) ) ;
#2183 = CARTESIAN_POINT ( 'NONE',  ( -83.29234334534424988, -124.7495837542614225, 2.751972736812206222 ) ) ;
#2184 = VERTEX_POINT ( 'NONE', #17783 ) ;
#2185 = VECTOR ( 'NONE', #2596, 1000.000000000000000 ) ;
#2186 = CARTESIAN_POINT ( 'NONE',  ( -82.17818763663338189, -125.4865065810072622, 7.120596377982462144 ) ) ;
#2187 = VECTOR ( 'NONE', #15931, 1000.000000000000000 ) ;
#2188 = FACE_OUTER_BOUND ( 'NONE', #14598, .T. ) ;
#2189 = LINE ( 'NONE', #5747, #15992 ) ;
#2190 = CARTESIAN_POINT ( 'NONE',  ( -122.8001410695374886, -86.14014948502065749, 39.99999999999999289 ) ) ;
#2191 = ORIENTED_EDGE ( 'NONE', *, *, #5529, .T. ) ;
#2192 = CIRCLE ( 'NONE', #12945, 62.91752772691707207 ) ;
#2193 = CARTESIAN_POINT ( 'NONE',  ( -137.1282911591921732, 23.88247324827570139, -17.14358333410968882 ) ) ;
#2194 = EDGE_LOOP ( 'NONE', ( #1180, #7572, #11325, #1194, #10826, #17173, #5243, #19202, #7135, #18239, #14187, #9679, #17719, #19543 ) ) ;
#2195 = CIRCLE ( 'NONE', #1189, 3.224098631618460331 ) ;
#2196 = VERTEX_POINT ( 'NONE', #288 ) ;
#2197 = EDGE_CURVE ( 'NONE', #4838, #15800, #3754, .T. ) ;
#2198 = AXIS2_PLACEMENT_3D ( 'NONE', #7177, #8698, #10324 ) ;
#2199 = DIRECTION ( 'NONE',  ( 6.982962677686266711E-15, -0.000000000000000000, 1.000000000000000000 ) ) ;
#2200 = CIRCLE ( 'NONE', #13267, 62.91752772691707207 ) ;
#2201 = DIRECTION ( 'NONE',  ( 1.000000000000000000, 0.000000000000000000, 0.000000000000000000 ) ) ;
#2202 = AXIS2_PLACEMENT_3D ( 'NONE', #11602, #11695, #16325 ) ;
#2203 = DIRECTION ( 'NONE',  ( 6.982962677686266711E-15, -0.000000000000000000, 1.000000000000000000 ) ) ;
#2204 = CARTESIAN_POINT ( 'NONE',  ( 0.8038475772933615371, 5.196152422706624030, -9.000000000000001776 ) ) ;
#2205 = CARTESIAN_POINT ( 'NONE',  ( 60.68773558783009747, -2.629322876227576433, 283.5832628385307999 ) ) ;
#2206 = CARTESIAN_POINT ( 'NONE',  ( -71.18887634719365565, -147.8252249328922687, 60.00000000000000000 ) ) ;
#2207 = CARTESIAN_POINT ( 'NONE',  ( -49.67518383744793908, 60.47951622432801599, 132.4711112102474146 ) ) ;
#2208 = CARTESIAN_POINT ( 'NONE',  ( 11.73417718768048701, 61.81362617575105389, 132.4711112102474146 ) ) ;
#2209 = CARTESIAN_POINT ( 'NONE',  ( 6.106329265062790945, -26.19668413589285194, 14.88498244535541026 ) ) ;
#2210 = CYLINDRICAL_SURFACE ( 'NONE', #11021, 60.74260934110282051 ) ;
#2211 = VERTEX_POINT ( 'NONE', #11225 ) ;
#2212 = VECTOR ( 'NONE', #12651, 1000.000000000000000 ) ;
#2213 = ORIENTED_EDGE ( 'NONE', *, *, #9199, .F. ) ;
#2215 = VERTEX_POINT ( 'NONE', #1930 ) ;
#2214 = AXIS2_PLACEMENT_3D ( 'NONE', #13685, #4382, #20133 ) ;
#2216 = VECTOR ( 'NONE', #15404, 1000.000000000000000 ) ;
#2217 = ORIENTED_EDGE ( 'NONE', *, *, #7018, .F. ) ;
#2218 = ORIENTED_EDGE ( 'NONE', *, *, #5166, .T. ) ;
#2219 = ADVANCED_FACE ( 'NONE', ( #8160, #3563 ), #14406, .F. ) ;
#2220 = EDGE_LOOP ( 'NONE', ( #965, #6524, #11975, #17424 ) ) ;
#2221 = LINE ( 'NONE', #6824, #4008 ) ;
#2222 = CARTESIAN_POINT ( 'NONE',  ( -58.69016442926522359, 0.8220851292433277724, 112.7772637782949516 ) ) ;
#2223 = DIRECTION ( 'NONE',  ( 1.000000000000000000, 0.000000000000000000, -0.000000000000000000 ) ) ;
#2224 = ORIENTED_EDGE ( 'NONE', *, *, #4993, .F. ) ;
#2225 = DIRECTION ( 'NONE',  ( -0.8830229359480271656, -0.4693298356057563625, 0.000000000000000000 ) ) ;
#2226 = DIRECTION ( 'NONE',  ( 0.000000000000000000, 0.000000000000000000, -1.000000000000000000 ) ) ;
#2227 = ORIENTED_EDGE ( 'NONE', *, *, #10835, .T. ) ;
#2228 = DIRECTION ( 'NONE',  ( -0.9396926207859114255, 0.3420201433256601642, 0.000000000000000000 ) ) ;
#2229 = ADVANCED_FACE ( 'NONE', ( #12862 ), #19118, .T. ) ;
#2230 = DIRECTION ( 'NONE',  ( 0.000000000000000000, 0.000000000000000000, -1.000000000000000000 ) ) ;
#2231 = DIRECTION ( 'NONE',  ( -1.000000000000000000, 0.000000000000000000, 0.000000000000000000 ) ) ;
#2232 = DIRECTION ( 'NONE',  ( -0.000000000000000000, -0.000000000000000000, 1.000000000000000000 ) ) ;
#2233 = CARTESIAN_POINT ( 'NONE',  ( -137.5516093427428359, -25.39430756190310845, -16.59029861066365541 ) ) ;
#2234 = DIRECTION ( 'NONE',  ( -0.000000000000000000, -0.000000000000000000, 1.000000000000000000 ) ) ;
#2235 = CARTESIAN_POINT ( 'NONE',  ( 0.000000000000000000, 0.000000000000000000, -10.00000000000000178 ) ) ;
#2236 = ORIENTED_EDGE ( 'NONE', *, *, #6635, .T. ) ;
#2237 = CARTESIAN_POINT ( 'NONE',  ( 0.000000000000000000, 0.000000000000000000, -100.0000000000000000 ) ) ;
#2238 = ORIENTED_EDGE ( 'NONE', *, *, #13967, .T. ) ;
#2239 = AXIS2_PLACEMENT_3D ( 'NONE', #7821, #13955, #17557 ) ;
#2240 = ORIENTED_EDGE ( 'NONE', *, *, #12488, .F. ) ;
#2241 = EDGE_CURVE ( 'NONE', #11142, #16800, #8256, .T. ) ;
#2242 = VECTOR ( 'NONE', #4721, 1000.000000000000000 ) ;
#2243 = CYLINDRICAL_SURFACE ( 'NONE', #12165, 99.99999999999997158 ) ;
#2244 = VECTOR ( 'NONE', #7986, 1000.000000000000000 ) ;
#2245 = ORIENTED_EDGE ( 'NONE', *, *, #15519, .T. ) ;
#2246 = CARTESIAN_POINT ( 'NONE',  ( 126.5370453525553671, 80.55045718954892209, 60.00000000000000000 ) ) ;
#2247 = CARTESIAN_POINT ( 'NONE',  ( -87.35350281426663344, -121.9411179691607146, 43.97512093379468467 ) ) ;
#2248 = CARTESIAN_POINT ( 'NONE',  ( -0.8220851292435327196, -58.69016442926522359, 132.4711112102474146 ) ) ;
#2249 = DIRECTION ( 'NONE',  ( 1.000000000000000000, 0.000000000000000000, 0.000000000000000000 ) ) ;
#2250 = ORIENTED_EDGE ( 'NONE', *, *, #5654, .F. ) ;
#2251 = EDGE_CURVE ( 'NONE', #12128, #7331, #354, .T. ) ;
#2252 = LINE ( 'NONE', #7901, #9997 ) ;
#2253 = CARTESIAN_POINT ( 'NONE',  ( 105.6231002115457329, -121.8324894761443886, 0.1248293295803034469 ) ) ;
#2254 = VECTOR ( 'NONE', #1710, 999.9999999999998863 ) ;
#2255 = VECTOR ( 'NONE', #17295, 1000.000000000000000 ) ;
#2256 = AXIS2_PLACEMENT_3D ( 'NONE', #2903, #17019, #2801 ) ;
#2257 = CARTESIAN_POINT ( 'NONE',  ( 0.000000000000000000, 0.000000000000000000, 49.99999999999999289 ) ) ;
#2258 = EDGE_CURVE ( 'NONE', #3545, #1477, #10380, .T. ) ;
#2259 = DIRECTION ( 'NONE',  ( 1.000000000000000000, 0.000000000000000000, -6.976128451377902853E-15 ) ) ;
#2260 = AXIS2_PLACEMENT_3D ( 'NONE', #3132, #9363, #15295 ) ;
#2261 = ORIENTED_EDGE ( 'NONE', *, *, #19165, .T. ) ;
#2262 = CARTESIAN_POINT ( 'NONE',  ( 43.41157826374501383, -91.36522714846361737, 14.88498244535515092 ) ) ;
#2263 = CARTESIAN_POINT ( 'NONE',  ( 59.30917539369505675, -13.12769224524051559, 293.5832628385307999 ) ) ;
#2264 = CARTESIAN_POINT ( 'NONE',  ( 30.25670013172214468, 55.16472960512381718, 248.9926560891072143 ) ) ;
#2265 = CARTESIAN_POINT ( 'NONE',  ( 56.12662799072089115, -23.22641211976269915, 283.5832628385307999 ) ) ;
#2266 = VERTEX_POINT ( 'NONE', #2331 ) ;
#2267 = CARTESIAN_POINT ( 'NONE',  ( 0.000000000000000000, 0.000000000000000000, 283.5832628385307999 ) ) ;
#2268 = DIRECTION ( 'NONE',  ( 0.000000000000000000, 0.000000000000000000, 1.000000000000000000 ) ) ;
#2269 = VERTEX_POINT ( 'NONE', #8950 ) ;
#2270 = B_SPLINE_CURVE_WITH_KNOTS ( 'NONE', 3,
 ( #6853, #3585, #2253, #608, #708, #9817, #6950, #5319, #12981, #5229, #11454, #19336, #16172, #7054, #13171, #2157, #19438, #8381, #5420, #2448, #11647, #3877, #10122, #16369 ),
 .UNSPECIFIED., .F., .F.,
 ( 4, 2, 2, 2, 2, 2, 2, 2, 2, 2, 2, 4 ),
 ( 0.000000000000000000, 0.005718059174761300212, 0.008577088762141958991, 0.01143611834952262124, 0.01286563314321295150, 0.01429514793690328175, 0.01715417752428397696, 0.01858369231797430202, 0.02001320711166462707, 0.02072796450850978092, 0.02144272190535493477, 0.02287223669904524595 ),
 .UNSPECIFIED. ) ;
#2271 = VERTEX_POINT ( 'NONE', #15194 ) ;
#2272 = EDGE_CURVE ( 'NONE', #10094, #5816, #16345, .T. ) ;
#2273 = VECTOR ( 'NONE', #9693, 1000.000000000000000 ) ;
#2274 = CIRCLE ( 'NONE', #9114, 32.50000000000000000 ) ;
#2275 = CARTESIAN_POINT ( 'NONE',  ( 18.28567271940513450, -57.92709869106715814, 293.5832628385307999 ) ) ;
#2276 = DIRECTION ( 'NONE',  ( 0.9511061040868794558, 0.3088643371590157338, 0.000000000000000000 ) ) ;
#2277 = EDGE_LOOP ( 'NONE', ( #15901, #13040, #15804, #4684 ) ) ;
#2278 = LINE ( 'NONE', #17634, #4022 ) ;
#2279 = FACE_BOUND ( 'NONE', #10646, .T. ) ;
#2280 = CARTESIAN_POINT ( 'NONE',  ( -96.05955731895396355, -115.3262050113649906, 4.792200876788737851 ) ) ;
#2281 = EDGE_LOOP ( 'NONE', ( #15820, #17001 ) ) ;
#2282 = ADVANCED_FACE ( 'NONE', ( #1072 ), #12016, .F. ) ;
#2283 = EDGE_CURVE ( 'NONE', #1965, #14511, #6892, .T. ) ;
#2284 = EDGE_CURVE ( 'NONE', #7600, #961, #10802, .T. ) ;
#2285 = DIRECTION ( 'NONE',  ( -1.000000000000000000, -3.491481338843133355E-15, 0.000000000000000000 ) ) ;
#2286 = DIRECTION ( 'NONE',  ( -0.1736481776669280275, 0.9848077530122084644, 1.076098267568195831E-15 ) ) ;
#2287 = FACE_OUTER_BOUND ( 'NONE', #13566, .T. ) ;
#2288 = DIRECTION ( 'NONE',  ( 0.000000000000000000, 0.000000000000000000, -1.000000000000000000 ) ) ;
#2289 = VECTOR ( 'NONE', #6610, 999.9999999999998863 ) ;
#2290 = DIRECTION ( 'NONE',  ( 0.7881095627315598540, 0.6155349844899715706, 0.000000000000000000 ) ) ;
#2291 = AXIS2_PLACEMENT_3D ( 'NONE', #12830, #1794, #19383 ) ;
#2292 = EDGE_LOOP ( 'NONE', ( #11795, #6552, #5825, #9650, #2390 ) ) ;
#2293 = CYLINDRICAL_SURFACE ( 'NONE', #10703, 99.99999999999997158 ) ;
#2294 = LINE ( 'NONE', #742, #4007 ) ;
#2295 = EDGE_CURVE ( 'NONE', #12285, #13478, #18672, .T. ) ;
#2296 = EDGE_LOOP ( 'NONE', ( #15493, #6815, #15055 ) ) ;
#2297 = VERTEX_POINT ( 'NONE', #7421 ) ;
#2298 = CIRCLE ( 'NONE', #4922, 160.0000000000000284 ) ;
#2299 = DIRECTION ( 'NONE',  ( -0.000000000000000000, -0.000000000000000000, 1.000000000000000000 ) ) ;
#2300 = CARTESIAN_POINT ( 'NONE',  ( -134.4038851132261527, -66.60439670040145188, 2.956331823707739836 ) ) ;
#2301 = CARTESIAN_POINT ( 'NONE',  ( 40.28046525994349736, 45.46865632508086463, 293.5832628385307999 ) ) ;
#2302 = ADVANCED_FACE ( 'NONE', ( #11913 ), #19800, .T. ) ;
#2303 = LINE ( 'NONE', #6999, #13247 ) ;
#2304 = CARTESIAN_POINT ( 'NONE',  ( 40.32479851956816930, -67.08601213326552681, 110.9660488491356887 ) ) ;
#2305 = LINE ( 'NONE', #8535, #630 ) ;
#2306 = CARTESIAN_POINT ( 'NONE',  ( -125.9311142016074427, -81.50627728740086297, -9.445171272693709597 ) ) ;
#2307 = CARTESIAN_POINT ( 'NONE',  ( 132.8875376985348851, -69.70168330571937076, 6.384740227332618367 ) ) ;
#2308 = DIRECTION ( 'NONE',  ( -6.982962677686266711E-15, 0.000000000000000000, -1.000000000000000000 ) ) ;
#2309 = FACE_OUTER_BOUND ( 'NONE', #7114, .T. ) ;
#2310 = EDGE_CURVE ( 'NONE', #6039, #2071, #7226, .T. ) ;
#2311 = ORIENTED_EDGE ( 'NONE', *, *, #8527, .F. ) ;
#2312 = AXIS2_PLACEMENT_3D ( 'NONE', #2757, #13686, #18408 ) ;
#2313 = CIRCLE ( 'NONE', #14729, 62.91752772691707207 ) ;
#2314 = ORIENTED_EDGE ( 'NONE', *, *, #5915, .F. ) ;
#2315 = VERTEX_POINT ( 'NONE', #16448 ) ;
#2316 = VERTEX_POINT ( 'NONE', #5797 ) ;
#2317 = CARTESIAN_POINT ( 'NONE',  ( -22.28973221005119854, -58.83691981461626597, 132.4711112102474146 ) ) ;
#2318 = ORIENTED_EDGE ( 'NONE', *, *, #14758, .F. ) ;
#2319 = CARTESIAN_POINT ( 'NONE',  ( 156.4179374840099683, -52.02840013023883614, 39.99999999999999289 ) ) ;
#2320 = VECTOR ( 'NONE', #4053, 1000.000000000000000 ) ;
#2321 = CARTESIAN_POINT ( 'NONE',  ( 0.000000000000000000, 0.000000000000000000, 283.5832628385307999 ) ) ;
#2322 = LINE ( 'NONE', #6827, #10687 ) ;
#2323 = ORIENTED_EDGE ( 'NONE', *, *, #16512, .F. ) ;
#2324 = CIRCLE ( 'NONE', #3933, 150.0000000000000284 ) ;
#2325 = CARTESIAN_POINT ( 'NONE',  ( -60.08127757648377809, -8.938941455415188031, 283.5832628385307999 ) ) ;
#2326 = FACE_OUTER_BOUND ( 'NONE', #14080, .T. ) ;
#2327 = ORIENTED_EDGE ( 'NONE', *, *, #17123, .F. ) ;
#2328 = DIRECTION ( 'NONE',  ( -0.000000000000000000, 0.000000000000000000, -1.000000000000000000 ) ) ;
#2329 = PLANE ( 'NONE',  #11328 ) ;
#2330 = CARTESIAN_POINT ( 'NONE',  ( -148.9554720520392834, -17.67108784863415138, 60.00000000000000000 ) ) ;
#2331 = CARTESIAN_POINT ( 'NONE',  ( 53.78543575132128751, 32.64570716507559212, 132.4711112102474146 ) ) ;
#2332 = DIRECTION ( 'NONE',  ( -0.03505990758545895342, -0.9993852124581886764, 0.000000000000000000 ) ) ;
#2333 = CARTESIAN_POINT ( 'NONE',  ( 138.2024300533213932, 89.85329105948596862, 49.99999999999999289 ) ) ;
#2334 = LINE ( 'NONE', #5907, #5129 ) ;
#2335 = ORIENTED_EDGE ( 'NONE', *, *, #16292, .F. ) ;
#2336 = CARTESIAN_POINT ( 'NONE',  ( -110.0000000000000142, 265.0000000000000000, -94.99999999999997158 ) ) ;
#2337 = ORIENTED_EDGE ( 'NONE', *, *, #2535, .T. ) ;
#2338 = VECTOR ( 'NONE', #15590, 1000.000000000000000 ) ;
#2339 = ORIENTED_EDGE ( 'NONE', *, *, #17111, .T. ) ;
#2340 = DIRECTION ( 'NONE',  ( 0.000000000000000000, 0.000000000000000000, -1.000000000000000000 ) ) ;
#2341 = VERTEX_POINT ( 'NONE', #5591 ) ;
#2342 = DIRECTION ( 'NONE',  ( -0.6234898018587431423, 0.7818314824680221431, 0.000000000000000000 ) ) ;
#2343 = FACE_OUTER_BOUND ( 'NONE', #8614, .T. ) ;
#2344 = CARTESIAN_POINT ( 'NONE',  ( 0.000000000000000000, 0.000000000000000000, -9.999999999999994671 ) ) ;
#2345 = LINE ( 'NONE', #8576, #18466 ) ;
#2346 = EDGE_LOOP ( 'NONE', ( #12795, #11604, #8860 ) ) ;
#2347 = FACE_OUTER_BOUND ( 'NONE', #11343, .T. ) ;
#2348 = DIRECTION ( 'NONE',  ( 0.000000000000000000, 0.000000000000000000, -1.000000000000000000 ) ) ;
#2349 = EDGE_CURVE ( 'NONE', #15754, #10590, #17356, .T. ) ;
#2350 = DIRECTION ( 'NONE',  ( 0.000000000000000000, 0.000000000000000000, -1.000000000000000000 ) ) ;
#2351 = DIRECTION ( 'NONE',  ( 0.000000000000000000, 0.000000000000000000, 1.000000000000000000 ) ) ;
#2352 = DIRECTION ( 'NONE',  ( 1.000000000000000000, 0.000000000000000000, 0.000000000000000000 ) ) ;
#2353 = VECTOR ( 'NONE', #15401, 999.9999999999998863 ) ;
#2354 = DIRECTION ( 'NONE',  ( -0.000000000000000000, -0.000000000000000000, 1.000000000000000000 ) ) ;
#2355 = DIRECTION ( 'NONE',  ( -0.000000000000000000, -0.000000000000000000, 1.000000000000000000 ) ) ;
#2356 = PLANE ( 'NONE',  #15439 ) ;
#2357 = ORIENTED_EDGE ( 'NONE', *, *, #10357, .F. ) ;
#2358 = FACE_OUTER_BOUND ( 'NONE', #6365, .T. ) ;
#2359 = CARTESIAN_POINT ( 'NONE',  ( 128.2779226595531270, 102.2982297021113141, 49.99999999999999289 ) ) ;
#2360 = ORIENTED_EDGE ( 'NONE', *, *, #5173, .F. ) ;
#2361 = EDGE_CURVE ( 'NONE', #5750, #5755, #1175, .T. ) ;
#2362 = VERTEX_POINT ( 'NONE', #16735 ) ;
#2363 = EDGE_CURVE ( 'NONE', #7427, #6858, #4254, .T. ) ;
#2364 = EDGE_CURVE ( 'NONE', #12693, #13684, #2725, .T. ) ;
#2365 = EDGE_CURVE ( 'NONE', #6701, #14795, #785, .T. ) ;
#2366 = PLANE ( 'NONE',  #7726 ) ;
#2367 = VECTOR ( 'NONE', #7281, 1000.000000000000000 ) ;
#2368 = ORIENTED_EDGE ( 'NONE', *, *, #3905, .T. ) ;
#2369 = VECTOR ( 'NONE', #1650, 1000.000000000000000 ) ;
#2370 = CARTESIAN_POINT ( 'NONE',  ( 95.44734317237649179, -116.0775604631400881, 7.549685134005517106 ) ) ;
#2371 = CARTESIAN_POINT ( 'NONE',  ( -96.60517994341971360, -114.8199649187100562, 3.756337634281994742 ) ) ;
#2372 = AXIS2_PLACEMENT_3D ( 'NONE', #11461, #15974, #14437 ) ;
#2373 = AXIS2_PLACEMENT_3D ( 'NONE', #14, #6162, #13605 ) ;
#2374 = ADVANCED_FACE ( 'NONE', ( #5495 ), #879, .F. ) ;
#2375 = CARTESIAN_POINT ( 'NONE',  ( 26.42151830275502178, 4.658826548058130790, 39.88498244535526993 ) ) ;
#2376 = DIRECTION ( 'NONE',  ( -0.9848077530122069101, -0.1736481776669374644, 0.000000000000000000 ) ) ;
#2377 = DIRECTION ( 'NONE',  ( -0.000000000000000000, -0.000000000000000000, 1.000000000000000000 ) ) ;
#2378 =( NAMED_UNIT ( * ) PLANE_ANGLE_UNIT ( ) SI_UNIT ( $, .RADIAN. ) );
#2379 = FACE_OUTER_BOUND ( 'NONE', #18234, .T. ) ;
#2380 = DIRECTION ( 'NONE',  ( -0.6427876096865328126, -0.7660444431189835646, 0.000000000000000000 ) ) ;
#2381 = ORIENTED_EDGE ( 'NONE', *, *, #13160, .F. ) ;
#2382 = CARTESIAN_POINT ( 'NONE',  ( -47.29944656917786006, -41.48948842197101783, 132.4711112102474146 ) ) ;
#2383 = LINE ( 'NONE', #13505, #4989 ) ;
#2384 = AXIS2_PLACEMENT_3D ( 'NONE', #19470, #1032, #13817 ) ;
#2385 = VECTOR ( 'NONE', #9210, 1000.000000000000000 ) ;
#2386 = ORIENTED_EDGE ( 'NONE', *, *, #11638, .F. ) ;
#2387 =( NAMED_UNIT ( * ) PLANE_ANGLE_UNIT ( ) SI_UNIT ( $, .RADIAN. ) );
#2388 = EDGE_CURVE ( 'NONE', #13281, #345, #2976, .T. ) ;
#2389 = CIRCLE ( 'NONE', #9248, 60.74260934110282051 ) ;
#2390 = ORIENTED_EDGE ( 'NONE', *, *, #8482, .T. ) ;
#2391 = EDGE_CURVE ( 'NONE', #11413, #3145, #18075, .T. ) ;
#2392 = CARTESIAN_POINT ( 'NONE',  ( 41.48948842197120257, -47.29944656917771795, 248.9926560891072143 ) ) ;
#2393 = EDGE_LOOP ( 'NONE', ( #8249, #12308, #8871, #7667 ) ) ;
#2394 = CARTESIAN_POINT ( 'NONE',  ( -12.28122767885804301, 61.70726652483831032, 293.5832628385307999 ) ) ;
#2395 = VECTOR ( 'NONE', #1636, 1000.000000000000114 ) ;
#2396 = DIRECTION ( 'NONE',  ( -0.8660254037844397068, 0.4999999999999978906, 0.000000000000000000 ) ) ;
#2397 = VECTOR ( 'NONE', #10548, 999.9999999999998863 ) ;
#2398 = PLANE ( 'NONE',  #7187 ) ;
#2399 = ORIENTED_EDGE ( 'NONE', *, *, #639, .T. ) ;
#2400 = DIRECTION ( 'NONE',  ( 0.000000000000000000, 0.000000000000000000, 1.000000000000000000 ) ) ;
#2401 = CARTESIAN_POINT ( 'NONE',  ( -122.8001410695374886, -86.14014948502065749, -9.999999999999998224 ) ) ;
#2402 = EDGE_CURVE ( 'NONE', #9431, #10259, #19626, .T. ) ;
#2403 = CARTESIAN_POINT ( 'NONE',  ( 132.5080654097352237, -70.41765848030621555, 4.966168250035042142 ) ) ;
#2404 = VECTOR ( 'NONE', #8646, 1000.000000000000000 ) ;
#2405 = DIRECTION ( 'NONE',  ( -0.000000000000000000, -0.000000000000000000, -1.000000000000000000 ) ) ;
#2406 = DIRECTION ( 'NONE',  ( 0.1390141521205946196, -0.9902903945359624593, 0.000000000000000000 ) ) ;
#2407 = ORIENTED_EDGE ( 'NONE', *, *, #11939, .T. ) ;
#2408 = AXIS2_PLACEMENT_3D ( 'NONE', #8178, #15859, #11038 ) ;
#2409 = VERTEX_POINT ( 'NONE', #12117 ) ;
#2410 = CIRCLE ( 'NONE', #7623, 30.00000000000000000 ) ;
#2411 = EDGE_LOOP ( 'NONE', ( #15328, #17475, #19860 ) ) ;
#2412 = ADVANCED_FACE ( 'NONE', ( #16837 ), #10580, .F. ) ;
#2413 = ADVANCED_FACE ( 'NONE', ( #20106 ), #12320, .F. ) ;
#2414 = VERTEX_POINT ( 'NONE', #6213 ) ;
#2415 = ORIENTED_EDGE ( 'NONE', *, *, #14270, .F. ) ;
#2416 = AXIS2_PLACEMENT_3D ( 'NONE', #829, #4097, #2675 ) ;
#2417 = EDGE_CURVE ( 'NONE', #15008, #14612, #3136, .T. ) ;
#2418 = FACE_OUTER_BOUND ( 'NONE', #11261, .T. ) ;
#2419 = PLANE ( 'NONE',  #7311 ) ;
#2420 = AXIS2_PLACEMENT_3D ( 'NONE', #12570, #15958, #6752 ) ;
#2421 = DIRECTION ( 'NONE',  ( -0.2225209339563047617, -0.9749279121818258398, 0.000000000000000000 ) ) ;
#2422 = ORIENTED_EDGE ( 'NONE', *, *, #19415, .T. ) ;
#2423 = EDGE_CURVE ( 'NONE', #16849, #2942, #4352, .T. ) ;
#2424 = DIRECTION ( 'NONE',  ( -0.000000000000000000, -0.000000000000000000, 1.000000000000000000 ) ) ;
#2425 = LINE ( 'NONE', #2517, #20217 ) ;
#2426 = VERTEX_POINT ( 'NONE', #17253 ) ;
#2427 = DIRECTION ( 'NONE',  ( -0.000000000000000000, -0.000000000000000000, 1.000000000000000000 ) ) ;
#2428 = CARTESIAN_POINT ( 'NONE',  ( 56.12853591711344592, -23.22718332831461652, 293.5832628385307999 ) ) ;
#2429 = CARTESIAN_POINT ( 'NONE',  ( -175.8776271403844191, -36.50981547337168109, 60.00000000000000000 ) ) ;
#2430 = DIRECTION ( 'NONE',  ( 1.000000000000000000, 0.000000000000000000, 0.000000000000000000 ) ) ;
#2431 = DIRECTION ( 'NONE',  ( -0.000000000000000000, -0.000000000000000000, -1.000000000000000000 ) ) ;
#2432 = CARTESIAN_POINT ( 'NONE',  ( -78.85162031257850401, -85.37653928070189124, 14.88498244535600357 ) ) ;
#2433 = ORIENTED_EDGE ( 'NONE', *, *, #5628, .T. ) ;
#2434 = LINE ( 'NONE', #14806, #18076 ) ;
#2435 = VECTOR ( 'NONE', #8325, 1000.000000000000000 ) ;
#2436 = ORIENTED_EDGE ( 'NONE', *, *, #1365, .T. ) ;
#2437 = ORIENTED_EDGE ( 'NONE', *, *, #13531, .F. ) ;
#2438 = FACE_OUTER_BOUND ( 'NONE', #6937, .T. ) ;
#2439 = VERTEX_POINT ( 'NONE', #9052 ) ;
#2440 = VERTEX_POINT ( 'NONE', #1290 ) ;
#2441 = LINE ( 'NONE', #18291, #10714 ) ;
#2442 = DIRECTION ( 'NONE',  ( 0.000000000000000000, 0.000000000000000000, 1.000000000000000000 ) ) ;
#2443 = CIRCLE ( 'NONE', #11896, 60.74260934110282051 ) ;
#2444 = CARTESIAN_POINT ( 'NONE',  ( -110.0000000000000142, 165.0000000000000000, 5.000000000000000888 ) ) ;
#2445 = DIRECTION ( 'NONE',  ( -0.000000000000000000, -0.000000000000000000, -1.000000000000000000 ) ) ;
#2446 = ORIENTED_EDGE ( 'NONE', *, *, #11970, .F. ) ;
#2447 = PLANE ( 'NONE',  #2829 ) ;
#2448 = CARTESIAN_POINT ( 'NONE',  ( 97.67856431661355998, -133.7203759155860894, 8.104337610931111158 ) ) ;
#2449 = DIRECTION ( 'NONE',  ( -1.000000000000000000, 0.000000000000000000, 0.000000000000000000 ) ) ;
#2450 = LINE ( 'NONE', #7249, #2780 ) ;
#2451 = ORIENTED_EDGE ( 'NONE', *, *, #19518, .F. ) ;
#2452 = FACE_OUTER_BOUND ( 'NONE', #7683, .T. ) ;
#2453 = FACE_OUTER_BOUND ( 'NONE', #19304, .T. ) ;
#2454 = VECTOR ( 'NONE', #10499, 1000.000000000000000 ) ;
#2455 = DIRECTION ( 'NONE',  ( -1.047444401652940164E-14, 1.000000000000000000, 0.000000000000000000 ) ) ;
#2456 = ORIENTED_EDGE ( 'NONE', *, *, #3733, .T. ) ;
#2457 = CARTESIAN_POINT ( 'NONE',  ( 150.0000000000000284, 1.836970198721029747E-14, 49.99999999999999289 ) ) ;
#2458 = PLANE ( 'NONE',  #6966 ) ;
#2459 = ORIENTED_EDGE ( 'NONE', *, *, #10492, .T. ) ;
#2460 = VECTOR ( 'NONE', #7444, 1000.000000000000114 ) ;
#2461 = ORIENTED_EDGE ( 'NONE', *, *, #4643, .T. ) ;
#2462 = CONTEXT_DEPENDENT_SHAPE_REPRESENTATION ( #18214, #11452 ) ;
#2463 = ORIENTED_EDGE ( 'NONE', *, *, #12973, .T. ) ;
#2464 = EDGE_CURVE ( 'NONE', #1862, #16627, #2003, .T. ) ;
#2465 = LINE ( 'NONE', #16778, #7493 ) ;
#2466 = CARTESIAN_POINT ( 'NONE',  ( -23.23469325536272478, -13.41455640552162443, 14.88498244535561454 ) ) ;
#2467 = ORIENTED_EDGE ( 'NONE', *, *, #14472, .T. ) ;
#2468 = CIRCLE ( 'NONE', #20097, 62.91752772691707207 ) ;
#2469 = CARTESIAN_POINT ( 'NONE',  ( -28.06281046684226155, 73.06915264522029929, 132.4711112102474146 ) ) ;
#2470 = CYLINDRICAL_SURFACE ( 'NONE', #11588, 60.74260934110282051 ) ;
#2471 = CARTESIAN_POINT ( 'NONE',  ( -137.5777631771917413, -26.05850252028229264, 26.56366211542366784 ) ) ;
#2472 = DIRECTION ( 'NONE',  ( 0.000000000000000000, 0.000000000000000000, 1.000000000000000000 ) ) ;
#2473 = DIRECTION ( 'NONE',  ( 0.000000000000000000, 0.000000000000000000, 1.000000000000000000 ) ) ;
#2474 = EDGE_CURVE ( 'NONE', #2923, #5289, #12531, .T. ) ;
#2475 = DIRECTION ( 'NONE',  ( 0.000000000000000000, 0.000000000000000000, 1.000000000000000000 ) ) ;
#2476 = DIRECTION ( 'NONE',  ( 0.5000000000000044409, 0.8660254037844360431, -3.228294802704586902E-15 ) ) ;
#2477 = CARTESIAN_POINT ( 'NONE',  ( -19.79297637435836421, 18.57624240429761642, 14.88498244535559145 ) ) ;
#2478 = DIRECTION ( 'NONE',  ( -0.9848077530122096857, 0.1736481776669206722, -0.000000000000000000 ) ) ;
#2479 = EDGE_LOOP ( 'NONE', ( #13804, #13370 ) ) ;
#2480 = ADVANCED_FACE ( 'NONE', ( #18584 ), #15299, .F. ) ;
#2481 = LINE ( 'NONE', #16309, #16284 ) ;
#2482 = DIRECTION ( 'NONE',  ( -6.982962677686266711E-15, 0.000000000000000000, -1.000000000000000000 ) ) ;
#2483 = CIRCLE ( 'NONE', #13907, 62.91752772691707207 ) ;
#2484 = ORIENTED_EDGE ( 'NONE', *, *, #786, .F. ) ;
#2485 = EDGE_LOOP ( 'NONE', ( #17362, #1686, #13782, #10159 ) ) ;
#2486 = EDGE_CURVE ( 'NONE', #1353, #1681, #14082, .T. ) ;
#2487 = DIRECTION ( 'NONE',  ( -1.000000000000000000, 0.000000000000000000, 0.000000000000000000 ) ) ;
#2488 = EDGE_LOOP ( 'NONE', ( #16772, #13380, #16877, #18182 ) ) ;
#2489 = LINE ( 'NONE', #2592, #1759 ) ;
#2490 = CIRCLE ( 'NONE', #13918, 7.500000000000006217 ) ;
#2491 = VECTOR ( 'NONE', #8817, 1000.000000000000000 ) ;
#2492 = CARTESIAN_POINT ( 'NONE',  ( -97.49999999999997158, -200.0000000000000000, 40.00000000000000000 ) ) ;
#2493 = LINE ( 'NONE', #14864, #17654 ) ;
#2494 = DIRECTION ( 'NONE',  ( -1.000000000000000000, -0.000000000000000000, -0.000000000000000000 ) ) ;
#2495 = FACE_OUTER_BOUND ( 'NONE', #15231, .T. ) ;
#2496 = AXIS2_PLACEMENT_3D ( 'NONE', #11129, #17390, #3567 ) ;
#2497 = EDGE_CURVE ( 'NONE', #9731, #10444, #20002, .T. ) ;
#2498 = LINE ( 'NONE', #4027, #11802 ) ;
#2499 = EDGE_CURVE ( 'NONE', #6452, #10937, #9506, .T. ) ;
#2500 = CYLINDRICAL_SURFACE ( 'NONE', #14085, 60.74260934110282051 ) ;
#2501 = DIRECTION ( 'NONE',  ( 6.982962677686266711E-15, 0.000000000000000000, 1.000000000000000000 ) ) ;
#2502 = CARTESIAN_POINT ( 'NONE',  ( -134.7221128596263782, -65.95429948960607192, 35.15983169740453462 ) ) ;
#2503 = VERTEX_POINT ( 'NONE', #4455 ) ;
#2504 = VECTOR ( 'NONE', #6931, 1000.000000000000000 ) ;
#2505 = EDGE_LOOP ( 'NONE', ( #15875, #17494, #284, #19923 ) ) ;
#2506 = AXIS2_PLACEMENT_3D ( 'NONE', #2466, #14836, #18114 ) ;
#2507 = EDGE_LOOP ( 'NONE', ( #426, #4398, #13594, #12738 ) ) ;
#2508 = ORIENTED_EDGE ( 'NONE', *, *, #3271, .T. ) ;
#2509 = CONICAL_SURFACE ( 'NONE', #10337, 34.99999999999997868, 0.7853981633974521648 ) ;
#2510 = EDGE_CURVE ( 'NONE', #13906, #6775, #15510, .T. ) ;
#2511 = ORIENTED_EDGE ( 'NONE', *, *, #5394, .T. ) ;
#2512 = CARTESIAN_POINT ( 'NONE',  ( -139.0134832045226290, -23.59969680251337820, 24.57866847611368755 ) ) ;
#2513 = DIRECTION ( 'NONE',  ( 6.982962677686266711E-15, -0.000000000000000000, 1.000000000000000000 ) ) ;
#2514 = DIRECTION ( 'NONE',  ( 0.000000000000000000, 0.000000000000000000, 1.000000000000000000 ) ) ;
#2515 = VERTEX_POINT ( 'NONE', #12431 ) ;
#2516 = CARTESIAN_POINT ( 'NONE',  ( 0.8038475772933646457, -10.39230484541326582, 2.804506490479260738E-17 ) ) ;
#2517 = CARTESIAN_POINT ( 'NONE',  ( -109.9999999999983515, 285.0000000000000568, 92.50000000000004263 ) ) ;
#2518 = ORIENTED_EDGE ( 'NONE', *, *, #13762, .F. ) ;
#2519 = FACE_OUTER_BOUND ( 'NONE', #19627, .T. ) ;
#2520 = DIRECTION ( 'NONE',  ( -6.982962677686266711E-15, 0.000000000000000000, -1.000000000000000000 ) ) ;
#2521 = CARTESIAN_POINT ( 'NONE',  ( 19.23614321207236699, -57.61627707419557964, 283.5832628385307999 ) ) ;
#2522 = ADVANCED_FACE ( 'NONE', ( #6314 ), #14073, .F. ) ;
#2523 = EDGE_CURVE ( 'NONE', #9872, #2821, #17153, .T. ) ;
#2524 = DIRECTION ( 'NONE',  ( 0.7660444431189749048, 0.6427876096865430267, 0.000000000000000000 ) ) ;
#2525 = EDGE_CURVE ( 'NONE', #10243, #10598, #19835, .T. ) ;
#2526 = EDGE_CURVE ( 'NONE', #19300, #241, #9056, .T. ) ;
#2527 = VECTOR ( 'NONE', #13993, 1000.000000000000000 ) ;
#2528 = CARTESIAN_POINT ( 'NONE',  ( 123.3142212418662922, -85.40728428760859003, 40.34936862486454601 ) ) ;
#2529 = CARTESIAN_POINT ( 'NONE',  ( -29.99999999999887379, 285.0000000000000568, -2.500000000000847766 ) ) ;
#2530 = ORIENTED_EDGE ( 'NONE', *, *, #1259, .T. ) ;
#2531 = DIRECTION ( 'NONE',  ( -0.7660444431189770143, 0.6427876096865404731, 5.348151281215661977E-15 ) ) ;
#2532 = EDGE_LOOP ( 'NONE', ( #16841, #13833, #9327, #7473 ) ) ;
#2533 = VERTEX_POINT ( 'NONE', #14180 ) ;
#2534 = LINE ( 'NONE', #19706, #14792 ) ;
#2535 = EDGE_CURVE ( 'NONE', #14190, #3818, #13623, .T. ) ;
#2536 = ORIENTED_EDGE ( 'NONE', *, *, #17351, .T. ) ;
#2537 = ORIENTED_EDGE ( 'NONE', *, *, #874, .T. ) ;
#2538 = CIRCLE ( 'NONE', #8424, 3.224098631618455890 ) ;
#2539 = DIRECTION ( 'NONE',  ( -0.4999999999999950040, -0.8660254037844415942, -0.000000000000000000 ) ) ;
#2540 = CIRCLE ( 'NONE', #3850, 150.0000000000000284 ) ;
#2541 = CARTESIAN_POINT ( 'NONE',  ( -86.50547518363038080, -122.5441694604242571, 42.98359700323086940 ) ) ;
#2542 = CYLINDRICAL_SURFACE ( 'NONE', #15883, 39.99999999999997868 ) ;
#2543 = CARTESIAN_POINT ( 'NONE',  ( -144.1130761623740568, -69.50842595698580340, 10.00000000000000178 ) ) ;
#2544 = ORIENTED_EDGE ( 'NONE', *, *, #14981, .T. ) ;
#2545 = CARTESIAN_POINT ( 'NONE',  ( -130.7962991791398792, -73.43504534872147360, 45.49776675456224950 ) ) ;
#2546 = DIRECTION ( 'NONE',  ( 0.000000000000000000, 0.000000000000000000, -1.000000000000000000 ) ) ;
#2547 = EDGE_CURVE ( 'NONE', #3721, #8371, #3538, .T. ) ;
#2548 = CARTESIAN_POINT ( 'NONE',  ( -29.99999999999887379, 275.0000000000000000, 12.49999999999916511 ) ) ;
#2549 = DIRECTION ( 'NONE',  ( 0.000000000000000000, 0.000000000000000000, 1.000000000000000000 ) ) ;
#2550 = CARTESIAN_POINT ( 'NONE',  ( -63.68887634719364144, -147.8252249328922687, 49.99999999999999289 ) ) ;
#2551 = CARTESIAN_POINT ( 'NONE',  ( 82.03125000000004263, -125.5821405433013780, 10.00000000000000178 ) ) ;
#2552 = DIRECTION ( 'NONE',  ( 1.000000000000000000, 1.047444401652940164E-14, 0.000000000000000000 ) ) ;
#2553 = AXIS2_PLACEMENT_3D ( 'NONE', #8742, #16438, #11428 ) ;
#2554 = ADVANCED_FACE ( 'NONE', ( #3334 ), #9574, .F. ) ;
#2555 = VERTEX_POINT ( 'NONE', #14581 ) ;
#2556 = CIRCLE ( 'NONE', #18580, 106.4288957539801004 ) ;
#2557 = FACE_OUTER_BOUND ( 'NONE', #18623, .T. ) ;
#2558 = FACE_BOUND ( 'NONE', #1286, .T. ) ;
#2559 = ORIENTED_EDGE ( 'NONE', *, *, #8365, .F. ) ;
#2560 = VERTEX_POINT ( 'NONE', #5184 ) ;
#2561 = DIRECTION ( 'NONE',  ( -0.000000000000000000, -0.000000000000000000, 1.000000000000000000 ) ) ;
#2562 = CARTESIAN_POINT ( 'NONE',  ( 3.304959094393253416, 31.03941509555038181, 14.88498244535543158 ) ) ;
#2563 = DIRECTION ( 'NONE',  ( -0.000000000000000000, -0.000000000000000000, 1.000000000000000000 ) ) ;
#2564 = ORIENTED_EDGE ( 'NONE', *, *, #4298, .T. ) ;
#2565 = CIRCLE ( 'NONE', #11390, 7.500000000000020428 ) ;
#2566 = CARTESIAN_POINT ( 'NONE',  ( 103.5848300920814751, -125.1657093462233945, 0.7932558400431272139 ) ) ;
#2567 = CARTESIAN_POINT ( 'NONE',  ( -99.73778183779744211, -112.0462389701484511, -10.00000000039103298 ) ) ;
#2568 = VECTOR ( 'NONE', #7390, 1000.000000000000000 ) ;
#2569 = AXIS2_PLACEMENT_3D ( 'NONE', #7492, #8182, #10554 ) ;
#2570 = CIRCLE ( 'NONE', #19562, 60.74260934110282051 ) ;
#2571 = CARTESIAN_POINT ( 'NONE',  ( -135.3256110043510034, -31.31229190813938956, -18.21647407188902434 ) ) ;
#2572 = PLANE ( 'NONE',  #4263 ) ;
#2573 = CARTESIAN_POINT ( 'NONE',  ( 0.000000000000000000, 0.000000000000000000, 293.5832628385307999 ) ) ;
#2574 = DIRECTION ( 'NONE',  ( -0.6427876096865379196, -0.7660444431189792347, 0.000000000000000000 ) ) ;
#2575 = LINE ( 'NONE', #9952, #2949 ) ;
#2576 = LINE ( 'NONE', #8807, #10203 ) ;
#2577 = LINE ( 'NONE', #13502, #11522 ) ;
#2578 = EDGE_CURVE ( 'NONE', #2923, #10487, #15266, .T. ) ;
#2579 = ORIENTED_EDGE ( 'NONE', *, *, #3781, .T. ) ;
#2580 = DIRECTION ( 'NONE',  ( -1.000000000000000000, 0.000000000000000000, 6.994638739193269649E-15 ) ) ;
#2581 = CARTESIAN_POINT ( 'NONE',  ( 9.564549117045078930, 62.18629025319817316, 293.5832628385307999 ) ) ;
#2582 = AXIS2_PLACEMENT_3D ( 'NONE', #4303, #12172, #10532 ) ;
#2583 = ORIENTED_EDGE ( 'NONE', *, *, #11704, .F. ) ;
#2584 = CIRCLE ( 'NONE', #12038, 7.500000000000002665 ) ;
#2585 = VECTOR ( 'NONE', #18915, 1000.000000000000000 ) ;
#2586 = AXIS2_PLACEMENT_3D ( 'NONE', #852, #7202, #14865 ) ;
#2587 = ORIENTED_EDGE ( 'NONE', *, *, #5242, .T. ) ;
#2588 = ORIENTED_EDGE ( 'NONE', *, *, #1138, .F. ) ;
#2589 = EDGE_CURVE ( 'NONE', #19558, #4614, #11097, .T. ) ;
#2590 = CARTESIAN_POINT ( 'NONE',  ( -49.24833719034228352, -60.83768308848361528, 248.9926560891072143 ) ) ;
#2591 = ORIENTED_EDGE ( 'NONE', *, *, #9613, .F. ) ;
#2592 = CARTESIAN_POINT ( 'NONE',  ( 13.12726406102080112, 59.30716253403179650, 283.5832628385307999 ) ) ;
#2593 = CARTESIAN_POINT ( 'NONE',  ( -109.5721339228237667, 31.03941509555038181, 14.88498244535621851 ) ) ;
#2594 = CARTESIAN_POINT ( 'NONE',  ( 17.50000000000001066, 0.000000000000000000, 4.999999999999948486 ) ) ;
#2595 = CARTESIAN_POINT ( 'NONE',  ( -96.59339607701299713, -114.7676973381553296, 49.52774819360320890 ) ) ;
#2596 = DIRECTION ( 'NONE',  ( 0.000000000000000000, 1.000000000000000000, -3.338476886082577323E-16 ) ) ;
#2597 = DIRECTION ( 'NONE',  ( 6.982962677686266711E-15, 0.000000000000000000, 1.000000000000000000 ) ) ;
#2598 = AXIS2_PLACEMENT_3D ( 'NONE', #15886, #17430, #3405 ) ;
#2599 = VECTOR ( 'NONE', #20201, 1000.000000000000000 ) ;
#2600 = ORIENTED_EDGE ( 'NONE', *, *, #11970, .T. ) ;
#2601 = FACE_OUTER_BOUND ( 'NONE', #13233, .T. ) ;
#2602 = CARTESIAN_POINT ( 'NONE',  ( 12.78021302872850562, -77.21438937758507848, 132.4711112102474146 ) ) ;
#2603 = CARTESIAN_POINT ( 'NONE',  ( -2.605298826210324936, -5.111158570922258448, 283.5832628385307999 ) ) ;
#2604 = FACE_OUTER_BOUND ( 'NONE', #5188, .T. ) ;
#2605 = CARTESIAN_POINT ( 'NONE',  ( 36.99514631729018532, -48.17959877923561862, 293.5832628385307999 ) ) ;
#2606 = CARTESIAN_POINT ( 'NONE',  ( 118.3534152657848608, 114.7431683447366595, 60.00000000000000000 ) ) ;
#2607 = EDGE_CURVE ( 'NONE', #14365, #6558, #9772, .T. ) ;
#2608 = ORIENTED_EDGE ( 'NONE', *, *, #12902, .T. ) ;
#2609 = EDGE_CURVE ( 'NONE', #12970, #8067, #17759, .T. ) ;
#2610 = ORIENTED_EDGE ( 'NONE', *, *, #19884, .F. ) ;
#2611 = VERTEX_POINT ( 'NONE', #5280 ) ;
#2612 = VERTEX_POINT ( 'NONE', #3436 ) ;
#2613 = EDGE_CURVE ( 'NONE', #12685, #17, #6713, .T. ) ;
#2614 = EDGE_LOOP ( 'NONE', ( #3626, #14039, #11730, #7222 ) ) ;
#2615 = EDGE_CURVE ( 'NONE', #6960, #12583, #569, .T. ) ;
#2616 = EDGE_CURVE ( 'NONE', #19796, #2833, #1217, .T. ) ;
#2617 = PLANE ( 'NONE',  #4715 ) ;
#2618 = DIRECTION ( 'NONE',  ( 0.000000000000000000, 1.000000000000000000, 0.000000000000000000 ) ) ;
#2619 = VERTEX_POINT ( 'NONE', #2108 ) ;
#2620 = LINE ( 'NONE', #14595, #9339 ) ;
#2621 = DIRECTION ( 'NONE',  ( 0.1736481776669340504, -0.9848077530122074652, 0.000000000000000000 ) ) ;
#2622 = ORIENTED_EDGE ( 'NONE', *, *, #15684, .T. ) ;
#2623 = LINE ( 'NONE', #6930, #20205 ) ;
#2624 = CIRCLE ( 'NONE', #17073, 7.500000000000020428 ) ;
#2625 = CARTESIAN_POINT ( 'NONE',  ( -17.24542129382105315, 20.55229278271246329, 39.88498244535557546 ) ) ;
#2626 = CARTESIAN_POINT ( 'NONE',  ( -134.7188131032332876, -72.93593548660989256, 9.503886819007655973 ) ) ;
#2627 =( GEOMETRIC_REPRESENTATION_CONTEXT ( 3 ) GLOBAL_UNCERTAINTY_ASSIGNED_CONTEXT ( ( #12345 ) ) GLOBAL_UNIT_ASSIGNED_CONTEXT ( ( #19961, #2387, #6276 ) ) REPRESENTATION_CONTEXT ( 'NONE', 'WORKASPACE' ) );
#2628 = CIRCLE ( 'NONE', #6555, 112.8770930172170495 ) ;
#2629 = CARTESIAN_POINT ( 'NONE',  ( 60.00000000000000711, 6.284666409917639535E-13, -115.0000000000000000 ) ) ;
#2630 = EDGE_CURVE ( 'NONE', #7170, #17394, #19295, .T. ) ;
#2631 = CARTESIAN_POINT ( 'NONE',  ( 132.7526696464367149, -84.67545766722484757, 39.11277240342198525 ) ) ;
#2632 = DIRECTION ( 'NONE',  ( 0.000000000000000000, 0.000000000000000000, 1.000000000000000000 ) ) ;
#2633 = ORIENTED_EDGE ( 'NONE', *, *, #12260, .T. ) ;
#2634 = LINE ( 'NONE', #8859, #18820 ) ;
#2635 = VERTEX_POINT ( 'NONE', #16023 ) ;
#2636 = EDGE_LOOP ( 'NONE', ( #12071, #6685, #2683, #19660 ) ) ;
#2637 = DIRECTION ( 'NONE',  ( 0.000000000000000000, 0.7071067811865447972, 0.7071067811865502373 ) ) ;
#2638 = VERTEX_POINT ( 'NONE', #11506 ) ;
#2639 = ORIENTED_EDGE ( 'NONE', *, *, #16795, .F. ) ;
#2640 = EDGE_CURVE ( 'NONE', #108, #15181, #12632, .T. ) ;
#2641 = VECTOR ( 'NONE', #8283, 1000.000000000000000 ) ;
#2642 = ADVANCED_FACE ( 'NONE', ( #12835 ), #19094, .F. ) ;
#2643 = ADVANCED_FACE ( 'NONE', ( #260 ), #14478, .F. ) ;
#2644 = CARTESIAN_POINT ( 'NONE',  ( 166.7850001792985495, -189.9999999999999432, 0.000000000000000000 ) ) ;
#2645 = PRESENTATION_STYLE_ASSIGNMENT (( #16656 ) ) ;
#2646 = CARTESIAN_POINT ( 'NONE',  ( -20.21777810286715749, -59.58067424803620327, 248.9926560891072143 ) ) ;
#2647 = CARTESIAN_POINT ( 'NONE',  ( -1.629865514042508456, -60.72073886220396588, 283.5832628385307999 ) ) ;
#2648 = DIRECTION ( 'NONE',  ( 0.2225209339563044841, 0.9749279121818258398, 0.000000000000000000 ) ) ;
#2649 = EDGE_LOOP ( 'NONE', ( #12745, #3338, #150, #10624, #6173, #3093 ) ) ;
#2650 = CARTESIAN_POINT ( 'NONE',  ( -55.62246070845768031, 18.77710619359134725, 111.4180192758973931 ) ) ;
#2651 = CARTESIAN_POINT ( 'NONE',  ( -109.9999999999983515, 285.0000000000000568, 85.00000000000001421 ) ) ;
#2652 = DIRECTION ( 'NONE',  ( 6.982962677686266711E-15, -0.000000000000000000, 1.000000000000000000 ) ) ;
#2653 = AXIS2_PLACEMENT_3D ( 'NONE', #6003, #20209, #1599 ) ;
#2654 = ORIENTED_EDGE ( 'NONE', *, *, #5991, .T. ) ;
#2655 = ADVANCED_FACE ( 'NONE', ( #17565 ), #18998, .T. ) ;
#2656 = DIRECTION ( 'NONE',  ( -0.000000000000000000, -0.000000000000000000, 1.000000000000000000 ) ) ;
#2657 = CARTESIAN_POINT ( 'NONE',  ( -133.6865796038707117, -79.84358686291113827, 37.46324078528252954 ) ) ;
#2658 = CARTESIAN_POINT ( 'NONE',  ( -73.82206860051547892, -25.99419088092166774, 248.9926560891072143 ) ) ;
#2659 = EDGE_LOOP ( 'NONE', ( #7483, #6678 ) ) ;
#2660 = FACE_OUTER_BOUND ( 'NONE', #2066, .T. ) ;
#2661 = PLANE ( 'NONE',  #20031 ) ;
#2662 = ORIENTED_EDGE ( 'NONE', *, *, #17555, .F. ) ;
#2663 = EDGE_LOOP ( 'NONE', ( #8353, #3788, #6370, #3707 ) ) ;
#2664 = CARTESIAN_POINT ( 'NONE',  ( 62.09913334491123038, 10.11498556985180208, 248.9926560891072143 ) ) ;
#2665 = EDGE_CURVE ( 'NONE', #807, #11267, #3835, .T. ) ;
#2666 = ADVANCED_FACE ( 'NONE', ( #467 ), #2210, .F. ) ;
#2667 = VERTEX_POINT ( 'NONE', #19679 ) ;
#2668 = DIRECTION ( 'NONE',  ( -1.000000000000000000, 0.000000000000000000, 0.000000000000000000 ) ) ;
#2669 = DIRECTION ( 'NONE',  ( 0.5300553768524375320, 0.8479630283625697595, 0.000000000000000000 ) ) ;
#2670 = ORIENTED_EDGE ( 'NONE', *, *, #11507, .T. ) ;
#2671 = CARTESIAN_POINT ( 'NONE',  ( 93.44030642264493736, -117.3428525121075268, -8.413488319981127006 ) ) ;
#2672 = CARTESIAN_POINT ( 'NONE',  ( -106.9434821670503339, -119.5159909196298997, -6.573008631163750622E-15 ) ) ;
#2673 = EDGE_CURVE ( 'NONE', #19329, #4234, #19485, .T. ) ;
#2674 = CARTESIAN_POINT ( 'NONE',  ( -136.3130597734152047, -31.14279861364121871, -13.33873441683735983 ) ) ;
#2675 = DIRECTION ( 'NONE',  ( 0.8660254037844432595, -0.4999999999999919509, 0.000000000000000000 ) ) ;
#2676 = CARTESIAN_POINT ( 'NONE',  ( -14.02132266220259460, 20.55229278271246329, 39.88498244535555415 ) ) ;
#2677 = CARTESIAN_POINT ( 'NONE',  ( 128.2779226595531270, 102.2982297021113141, 39.99999999999999289 ) ) ;
#2678 = CARTESIAN_POINT ( 'NONE',  ( 0.000000000000000000, 0.000000000000000000, 49.99999999999999289 ) ) ;
#2679 = DIRECTION ( 'NONE',  ( -0.7660444431189766812, 0.6427876096865408062, 5.380491337840978959E-15 ) ) ;
#2680 = ORIENTED_EDGE ( 'NONE', *, *, #4734, .T. ) ;
#2681 = LINE ( 'NONE', #13204, #19215 ) ;
#2682 = LINE ( 'NONE', #19756, #12827 ) ;
#2683 = ORIENTED_EDGE ( 'NONE', *, *, #11372, .F. ) ;
#2684 = ORIENTED_EDGE ( 'NONE', *, *, #18277, .T. ) ;
#2685 = CIRCLE ( 'NONE', #14117, 6.000000000000001776 ) ;
#2686 = ORIENTED_EDGE ( 'NONE', *, *, #874, .F. ) ;
#2687 = DIRECTION ( 'NONE',  ( -0.000000000000000000, -0.000000000000000000, 1.000000000000000000 ) ) ;
#2688 = ORIENTED_EDGE ( 'NONE', *, *, #1121, .T. ) ;
#2689 = CARTESIAN_POINT ( 'NONE',  ( 134.5348546532065654, -74.34984901039663896, 6.412720522032803849 ) ) ;
#2690 = CARTESIAN_POINT ( 'NONE',  ( 57.92709869106709419, 18.28567271940532990, 293.5832628385307999 ) ) ;
#2691 = CARTESIAN_POINT ( 'NONE',  ( 39.84224160888901167, 67.36461649554546227, 132.4711112102474146 ) ) ;
#2692 = DIRECTION ( 'NONE',  ( 0.000000000000000000, 0.000000000000000000, 1.000000000000000000 ) ) ;
#2693 = DIRECTION ( 'NONE',  ( 0.6155349844899687950, -0.7881095627315619634, 0.000000000000000000 ) ) ;
#2694 = LINE ( 'NONE', #16611, #1295 ) ;
#2695 = EDGE_LOOP ( 'NONE', ( #5244, #10996, #7052, #10335 ) ) ;
#2696 = LINE ( 'NONE', #7496, #3249 ) ;
#2697 = CARTESIAN_POINT ( 'NONE',  ( -135.0821395827941842, -65.21370709267439736, 8.503067959630589812 ) ) ;
#2698 = CARTESIAN_POINT ( 'NONE',  ( 134.1895921339707911, -76.75826352744203973, 4.256527938263594990 ) ) ;
#2699 = VECTOR ( 'NONE', #9999, 1000.000000000000114 ) ;
#2700 = VECTOR ( 'NONE', #10838, 1000.000000000000000 ) ;
#2701 = DIRECTION ( 'NONE',  ( 0.7430374143461878633, -0.6692498792541777819, 0.000000000000000000 ) ) ;
#2702 = DIRECTION ( 'NONE',  ( -0.000000000000000000, -0.000000000000000000, -1.000000000000000000 ) ) ;
#2703 = CARTESIAN_POINT ( 'NONE',  ( 0.000000000000000000, 0.000000000000000000, 132.4711112102474146 ) ) ;
#2704 = ORIENTED_EDGE ( 'NONE', *, *, #6449, .T. ) ;
#2705 = DIRECTION ( 'NONE',  ( 0.000000000000000000, 0.000000000000000000, 1.000000000000000000 ) ) ;
#2706 = AXIS2_PLACEMENT_3D ( 'NONE', #11654, #2455, #16573 ) ;
#2707 = ORIENTED_EDGE ( 'NONE', *, *, #11874, .T. ) ;
#2708 = ORIENTED_EDGE ( 'NONE', *, *, #9270, .T. ) ;
#2709 = ORIENTED_EDGE ( 'NONE', *, *, #9711, .T. ) ;
#2710 = VECTOR ( 'NONE', #10438, 1000.000000000000114 ) ;
#2711 = VECTOR ( 'NONE', #19308, 1000.000000000000114 ) ;
#2712 = ORIENTED_EDGE ( 'NONE', *, *, #660, .F. ) ;
#2713 = ADVANCED_FACE ( 'NONE', ( #2309 ), #11990, .T. ) ;
#2714 = LINE ( 'NONE', #18463, #10907 ) ;
#2715 = DIRECTION ( 'NONE',  ( 0.000000000000000000, 0.000000000000000000, 1.000000000000000000 ) ) ;
#2716 = ORIENTED_EDGE ( 'NONE', *, *, #1795, .T. ) ;
#2717 = AXIS2_PLACEMENT_3D ( 'NONE', #8569, #16157, #8370 ) ;
#2718 = CARTESIAN_POINT ( 'NONE',  ( 0.000000000000000000, 0.000000000000000000, 283.5832628385307999 ) ) ;
#2719 = DIRECTION ( 'NONE',  ( 0.000000000000000000, 0.000000000000000000, 1.000000000000000000 ) ) ;
#2720 = VERTEX_POINT ( 'NONE', #5377 ) ;
#2721 = CARTESIAN_POINT ( 'NONE',  ( -78.89303534320342237, 115.6558536819018030, -11.08742706010982104 ) ) ;
#2722 = DIRECTION ( 'NONE',  ( -6.982962677686266711E-15, 0.000000000000000000, -1.000000000000000000 ) ) ;
#2723 = CARTESIAN_POINT ( 'NONE',  ( 32.16802499836741447, 54.07248341783265033, 132.4711112102474146 ) ) ;
#2724 = VECTOR ( 'NONE', #18519, 1000.000000000000000 ) ;
#2725 = LINE ( 'NONE', #14894, #19946 ) ;
#2726 = UNCERTAINTY_MEASURE_WITH_UNIT (LENGTH_MEASURE( 1.000000000000000082E-05 ), #7973, 'distance_accuracy_value', 'NONE');
#2727 = EDGE_CURVE ( 'NONE', #10937, #7509, #17898, .T. ) ;
#2728 = CIRCLE ( 'NONE', #10226, 60.74260934110282051 ) ;
#2729 = EDGE_CURVE ( 'NONE', #17, #6819, #11889, .T. ) ;
#2730 = DIRECTION ( 'NONE',  ( 0.000000000000000000, 1.000000000000000000, 0.000000000000000000 ) ) ;
#2731 = DIRECTION ( 'NONE',  ( 0.8830229359480271656, 0.4693298356057563625, 0.000000000000000000 ) ) ;
#2732 = ORIENTED_EDGE ( 'NONE', *, *, #16984, .F. ) ;
#2733 = ADVANCED_FACE ( 'NONE', ( #8541 ), #5674, .F. ) ;
#2734 = CARTESIAN_POINT ( 'NONE',  ( 0.000000000000000000, 0.000000000000000000, 293.5832628385307999 ) ) ;
#2735 = VERTEX_POINT ( 'NONE', #18246 ) ;
#2736 = VECTOR ( 'NONE', #5458, 1000.000000000000227 ) ;
#2737 = ORIENTED_EDGE ( 'NONE', *, *, #2001, .F. ) ;
#2738 = FACE_OUTER_BOUND ( 'NONE', #2292, .T. ) ;
#2739 = VECTOR ( 'NONE', #13777, 1000.000000000000227 ) ;
#2740 = EDGE_LOOP ( 'NONE', ( #9606, #6657, #17889, #14634 ) ) ;
#2741 = ORIENTED_EDGE ( 'NONE', *, *, #11500, .F. ) ;
#2742 = ADVANCED_FACE ( 'NONE', ( #18149 ), #667, .F. ) ;
#2743 = PLANE ( 'NONE',  #15642 ) ;
#2744 = FACE_OUTER_BOUND ( 'NONE', #2969, .T. ) ;
#2745 = ORIENTED_EDGE ( 'NONE', *, *, #17241, .F. ) ;
#2746 = CARTESIAN_POINT ( 'NONE',  ( 60.22029172860436574, 7.948651060879242003, 283.5832628385307999 ) ) ;
#2747 = CARTESIAN_POINT ( 'NONE',  ( -140.0000000000000284, 1.714505518806295230E-14, 23.02775637731986436 ) ) ;
#2748 = EDGE_LOOP ( 'NONE', ( #5728, #2433, #15269, #10800 ) ) ;
#2749 = CARTESIAN_POINT ( 'NONE',  ( -133.7324673749508577, -67.93981414779142369, 39.50723089793449816 ) ) ;
#2750 = CARTESIAN_POINT ( 'NONE',  ( 51.24071425735604635, -32.61983739937743820, 283.5832628385307999 ) ) ;
#2751 = DIRECTION ( 'NONE',  ( 1.000000000000000000, 0.000000000000000000, 0.000000000000000000 ) ) ;
#2752 = ORIENTED_EDGE ( 'NONE', *, *, #9416, .T. ) ;
#2753 = EDGE_CURVE ( 'NONE', #11036, #9322, #8832, .T. ) ;
#2754 = VECTOR ( 'NONE', #9964, 1000.000000000000000 ) ;
#2755 = DIRECTION ( 'NONE',  ( -0.4999999999999919509, -0.8660254037844432595, 0.000000000000000000 ) ) ;
#2756 = EDGE_CURVE ( 'NONE', #6696, #17381, #14774, .T. ) ;
#2757 = CARTESIAN_POINT ( 'NONE',  ( 71.18887634719571622, -147.8252249328912740, 39.99999999999999289 ) ) ;
#2758 = DIRECTION ( 'NONE',  ( 0.000000000000000000, 0.000000000000000000, 1.000000000000000000 ) ) ;
#2759 = VERTEX_POINT ( 'NONE', #16425 ) ;
#2760 = ADVANCED_FACE ( 'NONE', ( #16619 ), #956, .F. ) ;
#2761 = LINE ( 'NONE', #9193, #598 ) ;
#2762 = FACE_OUTER_BOUND ( 'NONE', #5149, .T. ) ;
#2763 = EDGE_LOOP ( 'NONE', ( #13219, #15319, #17788, #14443 ) ) ;
#2764 = ORIENTED_EDGE ( 'NONE', *, *, #4402, .T. ) ;
#2765 = CARTESIAN_POINT ( 'NONE',  ( -98.15405843558684751, -133.0926928925743198, 33.62865000098088331 ) ) ;
#2766 = AXIS2_PLACEMENT_3D ( 'NONE', #9, #2980, #4405 ) ;
#2767 = ORIENTED_EDGE ( 'NONE', *, *, #762, .F. ) ;
#2768 = FACE_OUTER_BOUND ( 'NONE', #14640, .T. ) ;
#2769 = ADVANCED_FACE ( 'NONE', ( #4030 ), #3930, .F. ) ;
#2770 = DIRECTION ( 'NONE',  ( 0.3747554100459959958, 0.9271237148521535021, 0.000000000000000000 ) ) ;
#2771 = EDGE_LOOP ( 'NONE', ( #13142, #16829 ) ) ;
#2772 = LINE ( 'NONE', #17198, #6405 ) ;
#2773 = CARTESIAN_POINT ( 'NONE',  ( -41.06890862491506056, -47.66508197439456751, 293.5832628385307999 ) ) ;
#2774 = VECTOR ( 'NONE', #12270, 999.9999999999998863 ) ;
#2775 = CARTESIAN_POINT ( 'NONE',  ( 30.05702882063027914, 50.41613078340812848, 132.4711112102474146 ) ) ;
#2776 = CARTESIAN_POINT ( 'NONE',  ( 73.25972925305627825, -27.53920554013664912, 111.4180192758974499 ) ) ;
#2777 = CARTESIAN_POINT ( 'NONE',  ( 5.485913980968119219, -1.678175111358107374, 283.5832628385307999 ) ) ;
#2778 = DIRECTION ( 'NONE',  ( 0.7660444431189792347, -0.6427876096865379196, 0.000000000000000000 ) ) ;
#2779 = EDGE_CURVE ( 'NONE', #16780, #12002, #11792, .T. ) ;
#2780 = VECTOR ( 'NONE', #11649, 999.9999999999998863 ) ;
#2781 = CARTESIAN_POINT ( 'NONE',  ( 58.63718168490485283, 22.81000261549389307, 293.5832628385307999 ) ) ;
#2782 = EDGE_CURVE ( 'NONE', #818, #10937, #15071, .T. ) ;
#2783 = FACE_OUTER_BOUND ( 'NONE', #18255, .T. ) ;
#2784 = LINE ( 'NONE', #9005, #17741 ) ;
#2785 = EDGE_CURVE ( 'NONE', #10983, #8668, #10673, .T. ) ;
#2786 = VERTEX_POINT ( 'NONE', #5774 ) ;
#2787 = DIRECTION ( 'NONE',  ( -0.5300553768524375320, -0.8479630283625697595, 0.000000000000000000 ) ) ;
#2788 = CYLINDRICAL_SURFACE ( 'NONE', #8259, 60.74260934110282051 ) ;
#2789 = ORIENTED_EDGE ( 'NONE', *, *, #1601, .T. ) ;
#2790 = EDGE_CURVE ( 'NONE', #3549, #13282, #16580, .T. ) ;
#2791 = EDGE_LOOP ( 'NONE', ( #11971, #10201, #5018, #8038 ) ) ;
#2792 = VECTOR ( 'NONE', #3581, 1000.000000000000114 ) ;
#2793 = VERTEX_POINT ( 'NONE', #13529 ) ;
#2794 = FACE_BOUND ( 'NONE', #3280, .T. ) ;
#2795 = ADVANCED_FACE ( 'NONE', ( #6914 ), #13123, .F. ) ;
#2796 = ORIENTED_EDGE ( 'NONE', *, *, #6498, .F. ) ;
#2797 = DIRECTION ( 'NONE',  ( -0.9271237148521547233, 0.3747554100459928872, 0.000000000000000000 ) ) ;
#2798 = DIRECTION ( 'NONE',  ( 6.982962677686266711E-15, -0.000000000000000000, 1.000000000000000000 ) ) ;
#2799 = DIRECTION ( 'NONE',  ( -0.000000000000000000, -0.000000000000000000, -1.000000000000000000 ) ) ;
#2800 = DIRECTION ( 'NONE',  ( 0.7660444431189858960, -0.6427876096865300370, 0.000000000000000000 ) ) ;
#2801 = DIRECTION ( 'NONE',  ( -0.7660444431189858960, -0.6427876096865299260, 5.348151281215661977E-15 ) ) ;
#2802 = VECTOR ( 'NONE', #13870, 1000.000000000000114 ) ;
#2803 = EDGE_LOOP ( 'NONE', ( #18386, #6220, #1957 ) ) ;
#2804 = DIRECTION ( 'NONE',  ( 0.000000000000000000, 0.000000000000000000, -1.000000000000000000 ) ) ;
#2805 = CARTESIAN_POINT ( 'NONE',  ( -132.5095042660450986, -70.41495930836687478, 4.970722503819324345 ) ) ;
#2806 = CARTESIAN_POINT ( 'NONE',  ( 131.8028587768798161, -71.61967917965999675, -4.009458607015777609 ) ) ;
#2807 = CARTESIAN_POINT ( 'NONE',  ( 14.39940464655707331, 76.92888220842492331, 248.9926560891072143 ) ) ;
#2808 = COLOUR_RGB ( '', 0.08235294, 0.09019608, 0.10196078) ;
#2809 = DIRECTION ( 'NONE',  ( -0.000000000000000000, -1.000000000000000000, -0.000000000000000000 ) ) ;
#2810 = DIRECTION ( 'NONE',  ( 1.000000000000000000, 0.000000000000000000, 0.000000000000000000 ) ) ;
#2811 = VERTEX_POINT ( 'NONE', #2908 ) ;
#2812 = DIRECTION ( 'NONE',  ( -0.000000000000000000, -0.000000000000000000, 1.000000000000000000 ) ) ;
#2813 = ADVANCED_FACE ( 'NONE', ( #18559 ), #4540, .F. ) ;
#2814 = ORIENTED_EDGE ( 'NONE', *, *, #15802, .T. ) ;
#2815 = AXIS2_PLACEMENT_3D ( 'NONE', #9154, #12110, #4345 ) ;
#2816 = ORIENTED_EDGE ( 'NONE', *, *, #10850, .F. ) ;
#2817 = ORIENTED_EDGE ( 'NONE', *, *, #18917, .T. ) ;
#2818 = B_SPLINE_CURVE_WITH_KNOTS ( 'NONE', 3,
 ( #12812, #12606, #4854, #14149, #17339, #15996, #19171, #11283, #14254, #11385, #15895 ),
 .UNSPECIFIED., .F., .F.,
 ( 4, 2, 1, 2, 2, 4 ),
 ( -7.745966853365171458E-05, 0.001996111220376526555, 0.004069682109286705367, 0.008216823887107061256, 0.01651110744274777303, 0.03309967455402919312 ),
 .UNSPECIFIED. ) ;
#2819 = CARTESIAN_POINT ( 'NONE',  ( 78.68887634719573043, -147.8252249328912740, 49.99999999999999289 ) ) ;
#2820 = CARTESIAN_POINT ( 'NONE',  ( -107.4999999999999716, -200.0000000000000000, 40.00000000000000000 ) ) ;
#2821 = VERTEX_POINT ( 'NONE', #1470 ) ;
#2822 = DIRECTION ( 'NONE',  ( 0.000000000000000000, 0.000000000000000000, 1.000000000000000000 ) ) ;
#2823 = DIRECTION ( 'NONE',  ( 0.9396926207859058744, -0.3420201433256757628, -6.568644312862837946E-15 ) ) ;
#2824 = ORIENTED_EDGE ( 'NONE', *, *, #14008, .F. ) ;
#2825 = CARTESIAN_POINT ( 'NONE',  ( -83.39030327046282309, 111.1915035958187019, -17.74126483281444777 ) ) ;
#2826 = DIRECTION ( 'NONE',  ( -0.000000000000000000, -0.000000000000000000, 1.000000000000000000 ) ) ;
#2827 = CARTESIAN_POINT ( 'NONE',  ( -132.6188226329609847, -85.30892464212142556, 0.7282421557319730399 ) ) ;
#2828 = DIRECTION ( 'NONE',  ( 0.000000000000000000, 0.000000000000000000, -1.000000000000000000 ) ) ;
#2829 = AXIS2_PLACEMENT_3D ( 'NONE', #2650, #11646, #4275 ) ;
#2830 = AXIS2_PLACEMENT_3D ( 'NONE', #12441, #18906, #3149 ) ;
#2831 = CARTESIAN_POINT ( 'NONE',  ( 126.4587173007283667, -80.71184697945604114, 41.01728415539461992 ) ) ;
#2832 = DIRECTION ( 'NONE',  ( 0.9396926207859057634, -0.3420201433256758183, -6.456589605409169860E-15 ) ) ;
#2833 = VERTEX_POINT ( 'NONE', #16816 ) ;
#2834 = ADVANCED_FACE ( 'NONE', ( #15591 ), #4751, .T. ) ;
#2836 = ORIENTED_EDGE ( 'NONE', *, *, #14143, .T. ) ;
#2835 = AXIS2_PLACEMENT_3D ( 'NONE', #14804, #788, #17986 ) ;
#2837 = CARTESIAN_POINT ( 'NONE',  ( 13.12726406102079224, 59.30716253403178939, 283.5832628385307999 ) ) ;
#2838 = ORIENTED_EDGE ( 'NONE', *, *, #13359, .F. ) ;
#2839 = ORIENTED_EDGE ( 'NONE', *, *, #5666, .T. ) ;
#2840 = CARTESIAN_POINT ( 'NONE',  ( 61.98599999999999000, 0.000000000000000000, 0.000000000000000000 ) ) ;
#2841 = ORIENTED_EDGE ( 'NONE', *, *, #9752, .F. ) ;
#2842 = ORIENTED_EDGE ( 'NONE', *, *, #14623, .T. ) ;
#2843 = AXIS2_PLACEMENT_3D ( 'NONE', #10891, #18373, #13860 ) ;
#2844 = DIRECTION ( 'NONE',  ( 1.000000000000000000, 0.000000000000000000, 0.000000000000000000 ) ) ;
#2845 = EDGE_CURVE ( 'NONE', #10590, #12690, #3011, .T. ) ;
#2846 = DIRECTION ( 'NONE',  ( 0.000000000000000000, 0.000000000000000000, 1.000000000000000000 ) ) ;
#2847 = VERTEX_POINT ( 'NONE', #16920 ) ;
#2848 = DIRECTION ( 'NONE',  ( 0.000000000000000000, 0.000000000000000000, -1.000000000000000000 ) ) ;
#2849 = DIRECTION ( 'NONE',  ( 0.000000000000000000, 0.000000000000000000, 1.000000000000000000 ) ) ;
#2850 = ORIENTED_EDGE ( 'NONE', *, *, #3861, .T. ) ;
#2851 = VECTOR ( 'NONE', #13377, 1000.000000000000000 ) ;
#2852 = FACE_BOUND ( 'NONE', #12231, .T. ) ;
#2853 = LINE ( 'NONE', #10502, #19550 ) ;
#2854 = LINE ( 'NONE', #15324, #8004 ) ;
#2855 = DIRECTION ( 'NONE',  ( 0.000000000000000000, 0.000000000000000000, -1.000000000000000000 ) ) ;
#2856 = DIRECTION ( 'NONE',  ( 0.000000000000000000, 0.4999999999999998335, -0.8660254037844387076 ) ) ;
#2857 = CARTESIAN_POINT ( 'NONE',  ( 0.000000000000000000, -3.004629197474319246E-15, -9.000000000000000000 ) ) ;
#2858 = ORIENTED_EDGE ( 'NONE', *, *, #10082, .T. ) ;
#2859 = EDGE_CURVE ( 'NONE', #5289, #19124, #15274, .T. ) ;
#2860 = FACE_BOUND ( 'NONE', #7834, .T. ) ;
#2861 = CARTESIAN_POINT ( 'NONE',  ( 159.9599531637113330, -36.50981547336952104, 49.99999999999999289 ) ) ;
#2862 = EDGE_LOOP ( 'NONE', ( #14694, #5284, #9035, #19113 ) ) ;
#2863 = VERTEX_POINT ( 'NONE', #20083 ) ;
#2864 = DIRECTION ( 'NONE',  ( -1.000000000000000000, 0.000000000000000000, 0.000000000000000000 ) ) ;
#2865 = VECTOR ( 'NONE', #17692, 1000.000000000000000 ) ;
#2866 = AXIS2_PLACEMENT_3D ( 'NONE', #5902, #18376, #15818 ) ;
#2867 = ORIENTED_EDGE ( 'NONE', *, *, #5371, .T. ) ;
#2868 = DIRECTION ( 'NONE',  ( 0.000000000000000000, 0.000000000000000000, -1.000000000000000000 ) ) ;
#2869 = ADVANCED_FACE ( 'NONE', ( #5878 ), #12506, .F. ) ;
#2870 = DIRECTION ( 'NONE',  ( 1.000000000000000000, 1.047444401652940164E-14, 0.000000000000000000 ) ) ;
#2871 = ORIENTED_EDGE ( 'NONE', *, *, #19281, .F. ) ;
#2872 = CARTESIAN_POINT ( 'NONE',  ( 84.12762954502645130, -124.1876770196613222, 0.8036315111169505254 ) ) ;
#2873 = CARTESIAN_POINT ( 'NONE',  ( -100.7812499999999716, -111.0996833858562951, -6.938893903907228378E-15 ) ) ;
#2874 = ADVANCED_FACE ( 'NONE', ( #19877 ), #13943, .F. ) ;
#2875 = VECTOR ( 'NONE', #7513, 999.9999999999998863 ) ;
#2876 = CARTESIAN_POINT ( 'NONE',  ( -141.6670312114224828, -18.66040080199755380, -10.97841296083584517 ) ) ;
#2877 = CARTESIAN_POINT ( 'NONE',  ( 67.50000000000000000, 6.284666409917639535E-13, -115.0000000000000000 ) ) ;
#2878 = DIRECTION ( 'NONE',  ( -0.6718749999999991118, -0.7406645559057090100, -6.938893903907223447E-16 ) ) ;
#2879 = CARTESIAN_POINT ( 'NONE',  ( 0.000000000000000000, 0.000000000000000000, 49.99999999999999289 ) ) ;
#2880 = DIRECTION ( 'NONE',  ( 6.982962677686266711E-15, -0.000000000000000000, 1.000000000000000000 ) ) ;
#2881 = CARTESIAN_POINT ( 'NONE',  ( 84.96040761327756741, -123.6194689893705174, 40.73966003348574816 ) ) ;
#2882 = ORIENTED_EDGE ( 'NONE', *, *, #2729, .F. ) ;
#2883 = EDGE_CURVE ( 'NONE', #14190, #3030, #20188, .T. ) ;
#2884 = DIRECTION ( 'NONE',  ( -0.000000000000000000, -0.000000000000000000, 1.000000000000000000 ) ) ;
#2885 = DIRECTION ( 'NONE',  ( -0.6692498792541753394, -0.7430374143461900838, 0.000000000000000000 ) ) ;
#2886 = VERTEX_POINT ( 'NONE', #7500 ) ;
#2887 = VERTEX_POINT ( 'NONE', #9344 ) ;
#2888 = CARTESIAN_POINT ( 'NONE',  ( -109.9999999999994031, 292.9500000000000455, 85.00000000000000000 ) ) ;
#2889 = VECTOR ( 'NONE', #11447, 1000.000000000000000 ) ;
#2890 = VECTOR ( 'NONE', #15854, 1000.000000000000000 ) ;
#2891 = EDGE_LOOP ( 'NONE', ( #19002, #5002, #4917, #11329 ) ) ;
#2892 = AXIS2_PLACEMENT_3D ( 'NONE', #6574, #11259, #15770 ) ;
#2893 = FACE_OUTER_BOUND ( 'NONE', #3242, .T. ) ;
#2894 = ORIENTED_EDGE ( 'NONE', *, *, #8297, .F. ) ;
#2895 = EDGE_CURVE ( 'NONE', #18152, #959, #7397, .T. ) ;
#2896 = FACE_OUTER_BOUND ( 'NONE', #11235, .T. ) ;
#2897 = DIRECTION ( 'NONE',  ( -1.000000000000000000, 0.000000000000000000, 0.000000000000000000 ) ) ;
#2898 = ADVANCED_FACE ( 'NONE', ( #12409 ), #15378, .F. ) ;
#2899 = PRODUCT_RELATED_PRODUCT_CATEGORY ( 'part', '', ( #1474 ) ) ;
#2900 = LINE ( 'NONE', #4219, #4732 ) ;
#2901 = CARTESIAN_POINT ( 'NONE',  ( -77.50000000000000000, 9.491012693391988181E-15, -105.0000000000000142 ) ) ;
#2902 = LINE ( 'NONE', #13521, #2185 ) ;
#2903 = CARTESIAN_POINT ( 'NONE',  ( -103.8888757476053541, -46.65403860089418941, 14.88498244535617765 ) ) ;
#2904 = DIRECTION ( 'NONE',  ( -0.1736481776669172583, -0.9848077530122103518, -0.000000000000000000 ) ) ;
#2905 = DIRECTION ( 'NONE',  ( 0.000000000000000000, 0.000000000000000000, -1.000000000000000000 ) ) ;
#2906 = CARTESIAN_POINT ( 'NONE',  ( 132.3196846491737233, -70.65764850137227882, -3.065492718625203228 ) ) ;
#2907 = LINE ( 'NONE', #15377, #10157 ) ;
#2908 = CARTESIAN_POINT ( 'NONE',  ( -58.83691981461619491, 22.28973221005138683, 248.9926560891072143 ) ) ;
#2909 = CIRCLE ( 'NONE', #10735, 7.500000000000007105 ) ;
#2910 = CARTESIAN_POINT ( 'NONE',  ( -134.4924637689158260, -74.66092226662962617, 33.94378522399878761 ) ) ;
#2911 = AXIS2_PLACEMENT_3D ( 'NONE', #20183, #15963, #4534 ) ;
#2912 = ORIENTED_EDGE ( 'NONE', *, *, #19137, .T. ) ;
#2913 = VECTOR ( 'NONE', #10890, 1000.000000000000000 ) ;
#2914 = DIRECTION ( 'NONE',  ( 0.000000000000000000, 0.000000000000000000, 1.000000000000000000 ) ) ;
#2915 = EDGE_LOOP ( 'NONE', ( #4623, #8268, #6882, #17161 ) ) ;
#2916 = ORIENTED_EDGE ( 'NONE', *, *, #6756, .F. ) ;
#2917 = AXIS2_PLACEMENT_3D ( 'NONE', #13299, #10333, #11860 ) ;
#2918 = VERTEX_POINT ( 'NONE', #17128 ) ;
#2919 = ADVANCED_FACE ( 'NONE', ( #1368 ), #5979, .F. ) ;
#2920 = CIRCLE ( 'NONE', #1626, 7.500000000000002665 ) ;
#2921 = CARTESIAN_POINT ( 'NONE',  ( 62.95000000000000284, 0.000000000000000000, 0.000000000000000000 ) ) ;
#2922 = DIRECTION ( 'NONE',  ( 1.000000000000000000, 0.000000000000000000, 0.000000000000000000 ) ) ;
#2923 = VERTEX_POINT ( 'NONE', #14052 ) ;
#2924 = LINE ( 'NONE', #18685, #6749 ) ;
#2925 = CARTESIAN_POINT ( 'NONE',  ( 60.68773558783009747, -2.629322876227576433, 293.5832628385307999 ) ) ;
#2926 = ADVANCED_FACE ( 'NONE', ( #13632 ), #41, .F. ) ;
#2927 = ORIENTED_EDGE ( 'NONE', *, *, #11824, .T. ) ;
#2928 = CARTESIAN_POINT ( 'NONE',  ( 0.000000000000000000, 0.000000000000000000, 283.5832628385307999 ) ) ;
#2929 = CARTESIAN_POINT ( 'NONE',  ( 9.176097008933345123, -25.21111933077053990, 14.88498244535538895 ) ) ;
#2930 = FACE_OUTER_BOUND ( 'NONE', #5894, .T. ) ;
#2931 = APPLICATION_CONTEXT ( 'automotive_design' ) ;
#2932 = CARTESIAN_POINT ( 'NONE',  ( -22.30005961346265408, -56.50329132715937419, 283.5832628385307999 ) ) ;
#2933 = DIRECTION ( 'NONE',  ( 0.9396926207859105373, -0.3420201433256631063, 0.000000000000000000 ) ) ;
#2934 = DIRECTION ( 'NONE',  ( -0.8479630283625716469, 0.5300553768524345344, 0.000000000000000000 ) ) ;
#2935 = DIRECTION ( 'NONE',  ( 6.982962677686266711E-15, -0.000000000000000000, 1.000000000000000000 ) ) ;
#2936 = VECTOR ( 'NONE', #1641, 1000.000000000000000 ) ;
#2937 = AXIS2_PLACEMENT_3D ( 'NONE', #11804, #7124, #5792 ) ;
#2938 = ORIENTED_EDGE ( 'NONE', *, *, #7908, .F. ) ;
#2939 = ORIENTED_EDGE ( 'NONE', *, *, #346, .F. ) ;
#2940 = DIRECTION ( 'NONE',  ( 0.9396926207859104263, 0.3420201433256629953, -6.562243095054850434E-15 ) ) ;
#2941 = ORIENTED_EDGE ( 'NONE', *, *, #2525, .T. ) ;
#2942 = VERTEX_POINT ( 'NONE', #18453 ) ;
#2943 = DIRECTION ( 'NONE',  ( 0.000000000000000000, 0.000000000000000000, 1.000000000000000000 ) ) ;
#2944 = PRODUCT_DEFINITION_SHAPE ( 'NONE', 'NONE',  #20250 ) ;
#2945 = ORIENTED_EDGE ( 'NONE', *, *, #9252, .F. ) ;
#2946 = CARTESIAN_POINT ( 'NONE',  ( 55.43188410062170135, 19.30071112029698455, 132.4711112102474146 ) ) ;
#2947 = DIRECTION ( 'NONE',  ( 0.000000000000000000, 0.000000000000000000, -1.000000000000000000 ) ) ;
#2948 = FILL_AREA_STYLE_COLOUR ( '', #12204 ) ;
#2949 = VECTOR ( 'NONE', #15049, 1000.000000000000000 ) ;
#2950 = DIRECTION ( 'NONE',  ( 0.8660254037844397068, -0.4999999999999979461, -0.000000000000000000 ) ) ;
#2951 = ORIENTED_EDGE ( 'NONE', *, *, #9711, .F. ) ;
#2952 = VECTOR ( 'NONE', #733, 1000.000000000000000 ) ;
#2953 = CARTESIAN_POINT ( 'NONE',  ( 0.5590800469813600460, 5.620102221249812402, -8.265697409064610923 ) ) ;
#2954 = CARTESIAN_POINT ( 'NONE',  ( -12.11787020633453338, 60.78082026081703049, 248.9926560891072143 ) ) ;
#2955 = EDGE_LOOP ( 'NONE', ( #13923, #13203, #10488, #8012 ) ) ;
#2956 = FACE_BOUND ( 'NONE', #2043, .T. ) ;
#2957 = CARTESIAN_POINT ( 'NONE',  ( 0.000000000000000000, 0.000000000000000000, 39.99999999999999289 ) ) ;
#2958 = FACE_OUTER_BOUND ( 'NONE', #18422, .T. ) ;
#2959 = DIRECTION ( 'NONE',  ( 0.000000000000000000, 0.000000000000000000, 1.000000000000000000 ) ) ;
#2960 = CARTESIAN_POINT ( 'NONE',  ( -134.8030718230775449, -47.09494809331346232, 39.99999999999999289 ) ) ;
#2961 = CARTESIAN_POINT ( 'NONE',  ( -105.6803803075390107, 91.83969138069829796, 39.74985483127044006 ) ) ;
#2962 = VERTEX_POINT ( 'NONE', #12200 ) ;
#2963 = CARTESIAN_POINT ( 'NONE',  ( -32.61983739937760873, -51.24071425735591134, 283.5832628385307999 ) ) ;
#2964 = FACE_OUTER_BOUND ( 'NONE', #9152, .T. ) ;
#2965 = ORIENTED_EDGE ( 'NONE', *, *, #17308, .F. ) ;
#2966 = CIRCLE ( 'NONE', #9823, 40.00000000000000000 ) ;
#2967 = ORIENTED_EDGE ( 'NONE', *, *, #5286, .T. ) ;
#2968 = DIRECTION ( 'NONE',  ( 0.9511061040868794558, 0.3088643371590157338, 0.000000000000000000 ) ) ;
#2969 = EDGE_LOOP ( 'NONE', ( #6399, #16106, #14925, #16093 ) ) ;
#2970 = DIRECTION ( 'NONE',  ( -0.000000000000000000, -0.000000000000000000, -1.000000000000000000 ) ) ;
#2971 = DIRECTION ( 'NONE',  ( 1.000000000000000000, 0.000000000000000000, 0.000000000000000000 ) ) ;
#2972 = VERTEX_POINT ( 'NONE', #4436 ) ;
#2973 = CARTESIAN_POINT ( 'NONE',  ( 86.28560748592117591, -122.6989046848860596, -2.704177608915436792 ) ) ;
#2974 = DIRECTION ( 'NONE',  ( 0.1736481776669306920, -0.9848077530122080203, 0.000000000000000000 ) ) ;
#2975 = EDGE_CURVE ( 'NONE', #16978, #16987, #10665, .T. ) ;
#2976 = CIRCLE ( 'NONE', #4279, 7.500000000000020428 ) ;
#2977 = VECTOR ( 'NONE', #20187, 1000.000000000000000 ) ;
#2978 = DIRECTION ( 'NONE',  ( 0.000000000000000000, 0.000000000000000000, 1.000000000000000000 ) ) ;
#2979 = DIRECTION ( 'NONE',  ( 0.000000000000000000, 0.000000000000000000, 1.000000000000000000 ) ) ;
#2980 = DIRECTION ( 'NONE',  ( 0.000000000000000000, 0.000000000000000000, 1.000000000000000000 ) ) ;
#2981 = ORIENTED_EDGE ( 'NONE', *, *, #18155, .T. ) ;
#2982 = CARTESIAN_POINT ( 'NONE',  ( -113.3514208120937781, -17.29894464209964866, 14.88498244535624337 ) ) ;
#2983 = FACE_OUTER_BOUND ( 'NONE', #18034, .T. ) ;
#2984 = CARTESIAN_POINT ( 'NONE',  ( 0.000000000000000000, 0.000000000000000000, 269.6944534026102360 ) ) ;
#2985 = CARTESIAN_POINT ( 'NONE',  ( 82.84981732089829620, -125.0436758660689094, 35.85664428374888502 ) ) ;
#2986 = ORIENTED_EDGE ( 'NONE', *, *, #19843, .F. ) ;
#2987 = ADVANCED_FACE ( 'NONE', ( #11483, #9746 ), #1986, .T. ) ;
#2988 = CARTESIAN_POINT ( 'NONE',  ( -156.4179374840092862, -52.02840013024096066, 49.99999999999999289 ) ) ;
#2989 = CARTESIAN_POINT ( 'NONE',  ( 87.50000000000002842, -133.9542832461881119, 10.00000000000000178 ) ) ;
#2990 = ADVANCED_FACE ( 'NONE', ( #9553 ), #17543, .T. ) ;
#2991 = VERTEX_POINT ( 'NONE', #6593 ) ;
#2992 = EDGE_CURVE ( 'NONE', #18071, #18093, #3952, .T. ) ;
#2993 = VECTOR ( 'NONE', #17405, 1000.000000000000000 ) ;
#2994 = ORIENTED_EDGE ( 'NONE', *, *, #4392, .F. ) ;
#2995 = PRODUCT_CONTEXT ( 'NONE', #12986, 'mechanical' ) ;
#2996 = EDGE_LOOP ( 'NONE', ( #14290, #392, #6277, #2437 ) ) ;
#2997 = CARTESIAN_POINT ( 'NONE',  ( -97.83161216922238168, -133.5187961265288550, 7.436012734232853028 ) ) ;
#2998 = CARTESIAN_POINT ( 'NONE',  ( 0.000000000000000000, 65.74260934110282051, 293.5832628385307999 ) ) ;
#2999 = ORIENTED_EDGE ( 'NONE', *, *, #17501, .T. ) ;
#3000 = PLANE ( 'NONE',  #15796 ) ;
#3001 = CARTESIAN_POINT ( 'NONE',  ( 7.350000000000001421, 0.000000000000000000, 0.000000000000000000 ) ) ;
#3002 = EDGE_CURVE ( 'NONE', #3496, #6917, #17341, .T. ) ;
#3003 = LINE ( 'NONE', #19237, #3320 ) ;
#3004 = CARTESIAN_POINT ( 'NONE',  ( -88.01533840461537750, -121.4634816193508300, 44.65227205411735412 ) ) ;
#3005 = DIRECTION ( 'NONE',  ( -0.9848077530122097967, 0.1736481776669207000, 0.000000000000000000 ) ) ;
#3006 = CARTESIAN_POINT ( 'NONE',  ( -52.50000000000000000, -2.094888803305880013E-13, -105.0000000000000142 ) ) ;
#3007 = DIRECTION ( 'NONE',  ( -0.000000000000000000, -1.000000000000000000, -0.000000000000000000 ) ) ;
#3008 = CARTESIAN_POINT ( 'NONE',  ( -132.7769743428863194, -69.91161917917753499, 5.893941834771159627 ) ) ;
#3009 = CARTESIAN_POINT ( 'NONE',  ( 131.8276101104381155, -71.67687255337031615, 3.301485790455078728 ) ) ;
#3010 = CARTESIAN_POINT ( 'NONE',  ( 31.86742755225487045, 24.93940645478198803, 248.9926560891072143 ) ) ;
#3011 = LINE ( 'NONE', #6292, #19201 ) ;
#3012 = CARTESIAN_POINT ( 'NONE',  ( -132.2954651231983405, -86.73864221001061026, 39.54657277217020805 ) ) ;
#3013 = ORIENTED_EDGE ( 'NONE', *, *, #17507, .F. ) ;
#3014 = CARTESIAN_POINT ( 'NONE',  ( 0.000000000000000000, 0.000000000000000000, 248.9926560891072143 ) ) ;
#3015 = CIRCLE ( 'NONE', #18700, 7.500000000000007105 ) ;
#3016 = EDGE_CURVE ( 'NONE', #13254, #5912, #15388, .T. ) ;
#3017 = EDGE_CURVE ( 'NONE', #6900, #12395, #365, .T. ) ;
#3018 = EDGE_LOOP ( 'NONE', ( #7239, #4809, #7210, #12805 ) ) ;
#3019 = VERTEX_POINT ( 'NONE', #19173 ) ;
#3020 = ORIENTED_EDGE ( 'NONE', *, *, #14996, .T. ) ;
#3021 = B_SPLINE_CURVE_WITH_KNOTS ( 'NONE', 3,
 ( #3531, #13118, #3632, #16016, #17751, #11302, #659, #17559 ),
 .UNSPECIFIED., .F., .F.,
 ( 4, 2, 2, 4 ),
 ( 0.000000000000000000, 0.004946988332758800802, 0.007420482499138205540, 0.009893976665517610278 ),
 .UNSPECIFIED. ) ;
#3022 = EDGE_CURVE ( 'NONE', #6905, #19150, #19274, .T. ) ;
#3023 = DIRECTION ( 'NONE',  ( -0.000000000000000000, -0.000000000000000000, 1.000000000000000000 ) ) ;
#3024 = AXIS2_PLACEMENT_3D ( 'NONE', #7401, #5882, #12095 ) ;
#3025 = PLANE ( 'NONE',  #1579 ) ;
#3026 = ORIENTED_EDGE ( 'NONE', *, *, #6286, .F. ) ;
#3027 = AXIS2_PLACEMENT_3D ( 'NONE', #11859, #830, #3807 ) ;
#3028 = CARTESIAN_POINT ( 'NONE',  ( -139.7162331485264986, -5.470663635007961823, -13.49539711827200250 ) ) ;
#3029 = DIRECTION ( 'NONE',  ( -0.1390141521205912334, 0.9902903945359629034, 0.000000000000000000 ) ) ;
#3030 = VERTEX_POINT ( 'NONE', #8010 ) ;
#3031 = CARTESIAN_POINT ( 'NONE',  ( -92.41014453654959482, 99.55326438240551568, -25.26926237334177472 ) ) ;
#3032 = CARTESIAN_POINT ( 'NONE',  ( -4.340196821731034937E-15, 8.236864015571827125, -3.733333029993801233 ) ) ;
#3033 = CARTESIAN_POINT ( 'NONE',  ( -38.41834839689332171, 68.18670162478844077, 132.4711112102474146 ) ) ;
#3034 = AXIS2_PLACEMENT_3D ( 'NONE', #6695, #12916, #5164 ) ;
#3035 = DIRECTION ( 'NONE',  ( -0.000000000000000000, -0.000000000000000000, 1.000000000000000000 ) ) ;
#3036 = CARTESIAN_POINT ( 'NONE',  ( 9.176097008933519206, -25.21111933077053990, 39.88498244535539072 ) ) ;
#3037 = EDGE_CURVE ( 'NONE', #858, #1972, #9452, .T. ) ;
#3038 = CARTESIAN_POINT ( 'NONE',  ( 14.39940464655707331, 76.92888220842492331, 132.4711112102474146 ) ) ;
#3039 = PLANE ( 'NONE',  #1844 ) ;
#3040 = ADVANCED_FACE ( 'NONE', ( #19077 ), #139, .F. ) ;
#3041 = ORIENTED_EDGE ( 'NONE', *, *, #9659, .F. ) ;
#3042 = ORIENTED_EDGE ( 'NONE', *, *, #12123, .T. ) ;
#3043 = AXIS2_PLACEMENT_3D ( 'NONE', #15054, #5649, #6989 ) ;
#3044 = VECTOR ( 'NONE', #3203, 1000.000000000000227 ) ;
#3045 = ORIENTED_EDGE ( 'NONE', *, *, #4288, .T. ) ;
#3046 = ADVANCED_FACE ( 'NONE', ( #1877 ), #3212, .T. ) ;
#3047 = ORIENTED_EDGE ( 'NONE', *, *, #14000, .F. ) ;
#3048 = DIRECTION ( 'NONE',  ( 1.000000000000000000, 0.000000000000000000, 0.000000000000000000 ) ) ;
#3049 = ORIENTED_EDGE ( 'NONE', *, *, #10587, .F. ) ;
#3050 = FACE_OUTER_BOUND ( 'NONE', #13948, .T. ) ;
#3051 = TOROIDAL_SURFACE ( 'NONE', #12510, 160.0000000000000284, 10.00000000000000000 ) ;
#3052 = CARTESIAN_POINT ( 'NONE',  ( 0.000000000000000000, 0.000000000000000000, 283.5832628385307999 ) ) ;
#3053 = LINE ( 'NONE', #9177, #2739 ) ;
#3054 = DIRECTION ( 'NONE',  ( -0.1736481776669405452, -0.9848077530122062440, 1.214091813839188261E-15 ) ) ;
#3055 = ORIENTED_EDGE ( 'NONE', *, *, #5060, .F. ) ;
#3056 = CYLINDRICAL_SURFACE ( 'NONE', #11893, 3.224098631618457667 ) ;
#3057 = CARTESIAN_POINT ( 'NONE',  ( 0.000000000000000000, 0.000000000000000000, 293.5832628385307999 ) ) ;
#3058 = VERTEX_POINT ( 'NONE', #12609 ) ;
#3059 = CARTESIAN_POINT ( 'NONE',  ( 60.74260934110282051, 0.000000000000000000, 283.5832628385307999 ) ) ;
#3061 = AXIS2_PLACEMENT_3D ( 'NONE', #19028, #12562, #19125 ) ;
#3060 = PLANE ( 'NONE',  #14982 ) ;
#3062 = CYLINDRICAL_SURFACE ( 'NONE', #489, 9.999999999999994671 ) ;
#3063 = CARTESIAN_POINT ( 'NONE',  ( -29.99999999999887379, 265.0000000000000000, -2.500000000000847766 ) ) ;
#3064 = VECTOR ( 'NONE', #19377, 999.9999999999998863 ) ;
#3065 = CARTESIAN_POINT ( 'NONE',  ( -134.6416478978700297, -73.54075392783711607, 32.36000221440195190 ) ) ;
#3066 = CARTESIAN_POINT ( 'NONE',  ( -76.84700801462552988, 117.0241645140891364, 16.25045822160150166 ) ) ;
#3067 = VERTEX_POINT ( 'NONE', #5063 ) ;
#3068 = CARTESIAN_POINT ( 'NONE',  ( 113.3640620605769413, -25.59923667990641150, 14.88498244535466064 ) ) ;
#3069 =( GEOMETRIC_REPRESENTATION_CONTEXT ( 3 ) GLOBAL_UNCERTAINTY_ASSIGNED_CONTEXT ( ( #1073 ) ) GLOBAL_UNIT_ASSIGNED_CONTEXT ( ( #7638, #18491, #13564 ) ) REPRESENTATION_CONTEXT ( 'NONE', 'WORKASPACE' ) );
#3070 = EDGE_LOOP ( 'NONE', ( #18593, #11700, #19060 ) ) ;
#3071 = ORIENTED_EDGE ( 'NONE', *, *, #8404, .T. ) ;
#3072 = PLANE ( 'NONE',  #10075 ) ;
#3073 = VERTEX_POINT ( 'NONE', #14561 ) ;
#3074 = DIRECTION ( 'NONE',  ( 0.000000000000000000, 0.000000000000000000, 1.000000000000000000 ) ) ;
#3075 = CARTESIAN_POINT ( 'NONE',  ( 167.4599531637113330, -36.50981547336952104, 39.99999999999999289 ) ) ;
#3076 = ORIENTED_EDGE ( 'NONE', *, *, #174, .F. ) ;
#3077 = CIRCLE ( 'NONE', #8939, 3.224098631618458555 ) ;
#3078 = CARTESIAN_POINT ( 'NONE',  ( 82.03125000007472067, -125.5821405432526205, 9.254789121596214585 ) ) ;
#3079 = FACE_OUTER_BOUND ( 'NONE', #9975, .T. ) ;
#3080 = VECTOR ( 'NONE', #17274, 1000.000000000000000 ) ;
#3081 = DIRECTION ( 'NONE',  ( 0.6427876096865481337, -0.7660444431189707970, 0.000000000000000000 ) ) ;
#3082 = DIRECTION ( 'NONE',  ( 0.000000000000000000, 0.000000000000000000, 1.000000000000000000 ) ) ;
#3083 = EDGE_LOOP ( 'NONE', ( #10699, #7557, #17698, #16455 ) ) ;
#3084 = CARTESIAN_POINT ( 'NONE',  ( -27.93373560431178149, 14.53487841505308253, 248.9926560891072143 ) ) ;
#3085 = CARTESIAN_POINT ( 'NONE',  ( -55.62246070845768031, 18.77710619359134725, 132.4711112102474146 ) ) ;
#3086 = DIRECTION ( 'NONE',  ( -0.9396926207859057634, -0.3420201433256757073, 0.000000000000000000 ) ) ;
#3087 = CARTESIAN_POINT ( 'NONE',  ( 98.78543727593098822, -132.2400759706155782, 34.91745822596744375 ) ) ;
#3088 = VERTEX_POINT ( 'NONE', #4961 ) ;
#3089 = CARTESIAN_POINT ( 'NONE',  ( 7.950000000000000178, -5.196152422706607155, 8.999999999999998224 ) ) ;
#3090 = PLANE ( 'NONE',  #19379 ) ;
#3091 = ORIENTED_EDGE ( 'NONE', *, *, #13772, .T. ) ;
#3092 = ADVANCED_FACE ( 'NONE', ( #6794 ), #14361, .F. ) ;
#3093 = ORIENTED_EDGE ( 'NONE', *, *, #4161, .F. ) ;
#3094 = ORIENTED_EDGE ( 'NONE', *, *, #8335, .T. ) ;
#3095 = SHAPE_REPRESENTATION_RELATIONSHIP ( 'NONE' , 'NONE' ,  #15821, #17527 ) ;
#3096 = VERTEX_POINT ( 'NONE', #15798 ) ;
#3097 = DIRECTION ( 'NONE',  ( 0.2225209339563050392, 0.9749279121818257288, -0.000000000000000000 ) ) ;
#3098 = DIRECTION ( 'NONE',  ( -1.000000000000000000, 0.000000000000000000, -0.000000000000000000 ) ) ;
#3099 = ORIENTED_EDGE ( 'NONE', *, *, #14653, .F. ) ;
#3100 = CIRCLE ( 'NONE', #8366, 7.500000000000003553 ) ;
#3101 = LINE ( 'NONE', #15578, #9580 ) ;
#3102 = CARTESIAN_POINT ( 'NONE',  ( 10.11498556985161201, -62.09913334491128012, 132.4711112102474146 ) ) ;
#3103 = CARTESIAN_POINT ( 'NONE',  ( 127.8482905096654747, -78.45565238711300537, 48.39782711105171131 ) ) ;
#3104 = EDGE_CURVE ( 'NONE', #720, #4348, #1779, .T. ) ;
#3105 = CARTESIAN_POINT ( 'NONE',  ( -95.76651288691110153, -116.1232671447739335, 30.76217253845484834 ) ) ;
#3106 = AXIS2_PLACEMENT_3D ( 'NONE', #5207, #11436, #17690 ) ;
#3107 = CARTESIAN_POINT ( 'NONE',  ( -60.68567895461851691, 2.629250726500500956, 283.5832628385307999 ) ) ;
#3108 = FACE_OUTER_BOUND ( 'NONE', #10710, .T. ) ;
#3109 = EDGE_CURVE ( 'NONE', #11373, #4416, #14256, .T. ) ;
#3110 = FACE_OUTER_BOUND ( 'NONE', #6322, .T. ) ;
#3111 = CARTESIAN_POINT ( 'NONE',  ( -135.1060089021507906, -65.16414933482950289, 9.250158916602527981 ) ) ;
#3112 = CARTESIAN_POINT ( 'NONE',  ( 123.3088579007138748, -85.41493018851996055, -0.3457237010573973590 ) ) ;
#3113 = LINE ( 'NONE', #12090, #19962 ) ;
#3114 = DIRECTION ( 'NONE',  ( -0.8660254037844450359, 0.4999999999999889533, 0.000000000000000000 ) ) ;
#3115 = CARTESIAN_POINT ( 'NONE',  ( -129.0008258634001379, -76.61840651136952829, 40.10093462088531169 ) ) ;
#3116 = VERTEX_POINT ( 'NONE', #5257 ) ;
#3117 = LINE ( 'NONE', #12203, #86 ) ;
#3118 = AXIS2_PLACEMENT_3D ( 'NONE', #6152, #16989, #11143 ) ;
#3119 = EDGE_CURVE ( 'NONE', #9562, #315, #302, .T. ) ;
#3120 = ORIENTED_EDGE ( 'NONE', *, *, #14282, .T. ) ;
#3121 = AXIS2_PLACEMENT_3D ( 'NONE', #12815, #9747, #11286 ) ;
#3122 = VERTEX_POINT ( 'NONE', #16202 ) ;
#3123 = ORIENTED_EDGE ( 'NONE', *, *, #18630, .T. ) ;
#3124 = DIRECTION ( 'NONE',  ( -0.000000000000000000, -0.000000000000000000, -1.000000000000000000 ) ) ;
#3125 = EDGE_CURVE ( 'NONE', #11508, #15057, #9778, .T. ) ;
#3126 = CARTESIAN_POINT ( 'NONE',  ( -48.72193424476477475, -39.80940113486002474, 293.5832628385307999 ) ) ;
#3127 = VERTEX_POINT ( 'NONE', #3907 ) ;
#3128 = EDGE_CURVE ( 'NONE', #20118, #5750, #18937, .T. ) ;
#3129 = PRESENTATION_LAYER_ASSIGNMENT (  '', '', ( #10625 ) ) ;
#3130 = CARTESIAN_POINT ( 'NONE',  ( 0.000000000000000000, 0.000000000000000000, 132.4711112102474146 ) ) ;
#3131 = EDGE_CURVE ( 'NONE', #16066, #11398, #2189, .T. ) ;
#3132 = CARTESIAN_POINT ( 'NONE',  ( 0.000000000000000000, 60.00000000000000000, -115.0000000000000000 ) ) ;
#3133 = CARTESIAN_POINT ( 'NONE',  ( 0.000000000000000000, 0.000000000000000000, 248.9926560891072143 ) ) ;
#3134 = DIRECTION ( 'NONE',  ( 1.000000000000000000, 0.000000000000000000, -6.969309079188926949E-15 ) ) ;
#3135 = DIRECTION ( 'NONE',  ( 1.000000000000000000, 0.000000000000000000, 0.000000000000000000 ) ) ;
#3136 = LINE ( 'NONE', #13863, #7215 ) ;
#3137 = ORIENTED_EDGE ( 'NONE', *, *, #4494, .T. ) ;
#3138 = CARTESIAN_POINT ( 'NONE',  ( 50.41613078340802190, -30.05702882063045678, 132.4711112102474146 ) ) ;
#3139 = DIRECTION ( 'NONE',  ( 1.000000000000000000, 0.000000000000000000, 0.000000000000000000 ) ) ;
#3140 = CONICAL_SURFACE ( 'NONE', #8990, 9.000000000000000000, 1.047197551196600296 ) ;
#3141 = ORIENTED_EDGE ( 'NONE', *, *, #1905, .F. ) ;
#3142 = ORIENTED_EDGE ( 'NONE', *, *, #234, .T. ) ;
#3143 = EDGE_CURVE ( 'NONE', #10024, #7758, #13105, .T. ) ;
#3144 = EDGE_LOOP ( 'NONE', ( #12259, #6178, #2436, #10219 ) ) ;
#3145 = VERTEX_POINT ( 'NONE', #19652 ) ;
#3146 = AXIS2_PLACEMENT_3D ( 'NONE', #17379, #3352, #9591 ) ;
#3147 = FACE_OUTER_BOUND ( 'NONE', #11028, .T. ) ;
#3148 = ORIENTED_EDGE ( 'NONE', *, *, #14377, .T. ) ;
#3149 = DIRECTION ( 'NONE',  ( -0.03505990758545895342, -0.9993852124581886764, 0.000000000000000000 ) ) ;
#3150 = CARTESIAN_POINT ( 'NONE',  ( -101.1837452960046022, -128.8430157189652618, 37.75944112220433624 ) ) ;
#3151 = CARTESIAN_POINT ( 'NONE',  ( 0.8038475772933556529, -5.196152422706607155, 8.999999999999998224 ) ) ;
#3152 = LINE ( 'NONE', #17171, #15816 ) ;
#3153 = CYLINDRICAL_SURFACE ( 'NONE', #7761, 112.8770930172170210 ) ;
#3154 = ORIENTED_EDGE ( 'NONE', *, *, #8387, .F. ) ;
#3155 = EDGE_CURVE ( 'NONE', #18654, #14438, #11677, .T. ) ;
#3156 = FACE_OUTER_BOUND ( 'NONE', #9656, .T. ) ;
#3157 = CARTESIAN_POINT ( 'NONE',  ( 0.000000000000000000, -3.004629197474327134E-15, 9.000000000000000000 ) ) ;
#3158 = EDGE_CURVE ( 'NONE', #5389, #12640, #3712, .T. ) ;
#3159 = EDGE_CURVE ( 'NONE', #3030, #15236, #5353, .T. ) ;
#3160 = EDGE_LOOP ( 'NONE', ( #19301, #4729, #13376, #19732 ) ) ;
#3161 = VECTOR ( 'NONE', #11871, 1000.000000000000000 ) ;
#3162 = CARTESIAN_POINT ( 'NONE',  ( -77.82371257323825375, 127.0966514542041779, -18.77062444076983283 ) ) ;
#3163 = DIRECTION ( 'NONE',  ( -1.000000000000000000, 0.000000000000000000, 0.000000000000000000 ) ) ;
#3164 = CARTESIAN_POINT ( 'NONE',  ( -1.629937663769596368, -60.72279549541552512, 283.5832628385307999 ) ) ;
#3165 = CIRCLE ( 'NONE', #14589, 3.224098631618458555 ) ;
#3166 = DIRECTION ( 'NONE',  ( 0.9511061040868794558, 0.3088643371590157338, 0.000000000000000000 ) ) ;
#3167 = CARTESIAN_POINT ( 'NONE',  ( -75.89859996291112054, 117.6422707177539735, 13.05450749028729795 ) ) ;
#3168 = EDGE_LOOP ( 'NONE', ( #16357, #16408, #18289 ) ) ;
#3169 = CARTESIAN_POINT ( 'NONE',  ( -189.9999999999988916, 285.0000000000000568, 5.000000000000268230 ) ) ;
#3170 = ORIENTED_EDGE ( 'NONE', *, *, #6606, .F. ) ;
#3171 = CIRCLE ( 'NONE', #15227, 9.999999999999996447 ) ;
#3172 = ORIENTED_EDGE ( 'NONE', *, *, #7876, .T. ) ;
#3173 = LINE ( 'NONE', #9490, #2890 ) ;
#3174 = CIRCLE ( 'NONE', #14599, 7.500000000000000000 ) ;
#3175 = ORIENTED_EDGE ( 'NONE', *, *, #7651, .T. ) ;
#3176 = CARTESIAN_POINT ( 'NONE',  ( -118.4694476160224781, 78.16069504672601909, -34.09644551253335010 ) ) ;
#3177 = DIRECTION ( 'NONE',  ( 1.000000000000000000, 0.000000000000000000, 0.000000000000000000 ) ) ;
#3178 = VERTEX_POINT ( 'NONE', #8612 ) ;
#3179 = ADVANCED_FACE ( 'NONE', ( #2379 ), #10241, .F. ) ;
#3180 = CARTESIAN_POINT ( 'NONE',  ( 96.25732604711784290, -115.9704170962574352, 9.968274243565256043 ) ) ;
#3181 = CYLINDRICAL_SURFACE ( 'NONE', #3762, 60.74260934110282051 ) ;
#3182 = EDGE_CURVE ( 'NONE', #19763, #15222, #8517, .T. ) ;
#3183 = FACE_OUTER_BOUND ( 'NONE', #6040, .T. ) ;
#3184 = DIRECTION ( 'NONE',  ( -1.000000000000000000, 0.000000000000000000, 0.000000000000000000 ) ) ;
#3185 = ORIENTED_EDGE ( 'NONE', *, *, #11384, .T. ) ;
#3186 = DIRECTION ( 'NONE',  ( -0.2080686897406943958, -0.9781142164131909622, 0.000000000000000000 ) ) ;
#3187 = DIRECTION ( 'NONE',  ( 1.000000000000000000, 0.000000000000000000, 0.000000000000000000 ) ) ;
#3188 = CARTESIAN_POINT ( 'NONE',  ( 0.000000000000000000, 0.000000000000000000, 293.5832628385307999 ) ) ;
#3189 = CARTESIAN_POINT ( 'NONE',  ( 85.70335357680444588, -123.1056148428117183, 41.89337921544904475 ) ) ;
#3190 = ORIENTED_EDGE ( 'NONE', *, *, #7762, .T. ) ;
#3191 = AXIS2_PLACEMENT_3D ( 'NONE', #9188, #5107, #10924 ) ;
#3192 = DIRECTION ( 'NONE',  ( 0.000000000000000000, 0.000000000000000000, 1.000000000000000000 ) ) ;
#3193 = DIRECTION ( 'NONE',  ( -0.9396926207859082059, -0.3420201433256694901, 0.000000000000000000 ) ) ;
#3194 = AXIS2_PLACEMENT_3D ( 'NONE', #15486, #17025, #18351 ) ;
#3195 = ORIENTED_EDGE ( 'NONE', *, *, #8308, .T. ) ;
#3196 = EDGE_LOOP ( 'NONE', ( #17005, #17105, #18751, #747, #18294, #2069 ) ) ;
#3197 = ORIENTED_EDGE ( 'NONE', *, *, #12775, .T. ) ;
#3198 = DIRECTION ( 'NONE',  ( 1.000000000000000000, 0.000000000000000000, 0.000000000000000000 ) ) ;
#3199 = VERTEX_POINT ( 'NONE', #644 ) ;
#3200 = CARTESIAN_POINT ( 'NONE',  ( -107.4999999999999858, -118.5063289449133777, 0.000000000000000000 ) ) ;
#3201 = FACE_BOUND ( 'NONE', #761, .T. ) ;
#3202 = VERTEX_POINT ( 'NONE', #2477 ) ;
#3203 = DIRECTION ( 'NONE',  ( -0.4693298356057531429, 0.8830229359480288309, 0.000000000000000000 ) ) ;
#3204 = CARTESIAN_POINT ( 'NONE',  ( -22.28973221005119854, -58.83691981461626597, 293.5832628385307999 ) ) ;
#3205 = CARTESIAN_POINT ( 'NONE',  ( -82.18957362175343917, -125.4791168306735329, 7.014959006335095282 ) ) ;
#3206 = VECTOR ( 'NONE', #4105, 1000.000000000000114 ) ;
#3207 = CARTESIAN_POINT ( 'NONE',  ( -91.89277925369268019, -118.5585056022070063, 47.62084010467887651 ) ) ;
#3208 = DIRECTION ( 'NONE',  ( 1.000000000000000000, 0.000000000000000000, -6.977185866873309606E-15 ) ) ;
#3209 = CARTESIAN_POINT ( 'NONE',  ( -138.6697530361317945, 19.64131382463628839, 25.10535822172604270 ) ) ;
#3210 = DIRECTION ( 'NONE',  ( 0.000000000000000000, 0.000000000000000000, 1.000000000000000000 ) ) ;
#3211 = DIRECTION ( 'NONE',  ( -0.7660444431189858960, 0.6427876096865300370, 0.000000000000000000 ) ) ;
#3212 = CYLINDRICAL_SURFACE ( 'NONE', #5592, 3.224098631618457667 ) ;
#3213 = CARTESIAN_POINT ( 'NONE',  ( -132.4144148200023778, -86.21736781321662590, 39.45061808899835398 ) ) ;
#3214 = ORIENTED_EDGE ( 'NONE', *, *, #14917, .F. ) ;
#3215 = DIRECTION ( 'NONE',  ( 0.000000000000000000, 0.000000000000000000, 1.000000000000000000 ) ) ;
#3216 = VECTOR ( 'NONE', #15911, 1000.000000000000000 ) ;
#3217 = VECTOR ( 'NONE', #7258, 1000.000000000000114 ) ;
#3218 = ORIENTED_EDGE ( 'NONE', *, *, #12083, .F. ) ;
#3219 = VERTEX_POINT ( 'NONE', #16306 ) ;
#3220 = VERTEX_POINT ( 'NONE', #6888 ) ;
#3221 = DIRECTION ( 'NONE',  ( -0.000000000000000000, -0.000000000000000000, 1.000000000000000000 ) ) ;
#3222 = DIRECTION ( 'NONE',  ( -0.000000000000000000, -0.000000000000000000, 1.000000000000000000 ) ) ;
#3223 = VECTOR ( 'NONE', #74, 1000.000000000000000 ) ;
#3224 = DIRECTION ( 'NONE',  ( 1.000000000000000000, 0.000000000000000000, -6.976128451377903642E-15 ) ) ;
#3225 = AXIS2_PLACEMENT_3D ( 'NONE', #18622, #18315, #4291 ) ;
#3226 = EDGE_CURVE ( 'NONE', #10982, #16530, #10746, .T. ) ;
#3227 = DIRECTION ( 'NONE',  ( 1.000000000000000000, 0.000000000000000000, -6.994638739193269649E-15 ) ) ;
#3228 = VECTOR ( 'NONE', #565, 1000.000000000000000 ) ;
#3229 = ADVANCED_FACE ( 'NONE', ( #16398 ), #15050, .T. ) ;
#3230 = DIRECTION ( 'NONE',  ( 6.982962677686266711E-15, 0.000000000000000000, 1.000000000000000000 ) ) ;
#3231 = CARTESIAN_POINT ( 'NONE',  ( 120.7779226595530986, 102.2982297021113141, 60.00000000000000000 ) ) ;
#3232 = CARTESIAN_POINT ( 'NONE',  ( -76.92888220842476699, 14.39940464655786201, 248.9926560891072143 ) ) ;
#3233 = DIRECTION ( 'NONE',  ( 0.000000000000000000, 0.000000000000000000, 1.000000000000000000 ) ) ;
#3234 = ORIENTED_EDGE ( 'NONE', *, *, #4154, .T. ) ;
#3235 = B_SPLINE_CURVE_WITH_KNOTS ( 'NONE', 3,
 ( #12063, #18327, #7470, #20160, #19850, #1232 ),
 .UNSPECIFIED., .F., .F.,
 ( 4, 2, 4 ),
 ( 0.009719890944573138583, 0.01235036185894304236, 0.01498083277331294441 ),
 .UNSPECIFIED. ) ;
#3236 = CARTESIAN_POINT ( 'NONE',  ( 134.6900874600792122, -73.16343714251466679, 31.49281596304311748 ) ) ;
#3237 = ADVANCED_FACE ( 'NONE', ( #831 ), #6984, .T. ) ;
#3238 = CARTESIAN_POINT ( 'NONE',  ( 133.6841479863219888, -79.85751371701381629, 37.46951788548890505 ) ) ;
#3239 = ORIENTED_EDGE ( 'NONE', *, *, #7352, .F. ) ;
#3240 = ORIENTED_EDGE ( 'NONE', *, *, #7995, .T. ) ;
#3241 = EDGE_CURVE ( 'NONE', #13065, #12180, #18124, .T. ) ;
#3242 = EDGE_LOOP ( 'NONE', ( #10222, #5250, #13945, #15544 ) ) ;
#3243 = ADVANCED_FACE ( 'NONE', ( #7276 ), #7083, .T. ) ;
#3244 = AXIS2_PLACEMENT_3D ( 'NONE', #6130, #11124, #10920 ) ;
#3245 = VECTOR ( 'NONE', #14198, 1000.000000000000000 ) ;
#3246 = ORIENTED_EDGE ( 'NONE', *, *, #3297, .F. ) ;
#3247 = EDGE_CURVE ( 'NONE', #11476, #244, #14944, .T. ) ;
#3248 = CARTESIAN_POINT ( 'NONE',  ( -1.629937663769596368, -60.72279549541552512, 293.5832628385307999 ) ) ;
#3249 = VECTOR ( 'NONE', #11986, 1000.000000000000000 ) ;
#3250 = ORIENTED_EDGE ( 'NONE', *, *, #17244, .F. ) ;
#3251 = LINE ( 'NONE', #13977, #14909 ) ;
#3252 = PLANE ( 'NONE',  #4338 ) ;
#3253 = CARTESIAN_POINT ( 'NONE',  ( 0.000000000000000000, 60.00000000000000000, -115.0000000000000000 ) ) ;
#3254 = CARTESIAN_POINT ( 'NONE',  ( -32.50000000000000000, 3.980102097228898626E-15, -115.0000000000000000 ) ) ;
#3255 = DIRECTION ( 'NONE',  ( -0.000000000000000000, -0.000000000000000000, 1.000000000000000000 ) ) ;
#3256 = VERTEX_POINT ( 'NONE', #16591 ) ;
#3257 = CARTESIAN_POINT ( 'NONE',  ( 128.9113527779074673, -76.70395394680461720, -7.603355451428101652 ) ) ;
#3258 = CARTESIAN_POINT ( 'NONE',  ( 0.07661102881317774504, 6.914460432017340175, 6.023803224821316249 ) ) ;
#3259 = EDGE_CURVE ( 'NONE', #3019, #3346, #2576, .T. ) ;
#3260 = VERTEX_POINT ( 'NONE', #10434 ) ;
#3261 = PLANE ( 'NONE',  #16872 ) ;
#3262 = CARTESIAN_POINT ( 'NONE',  ( -110.0000000000000142, 275.0000000000000000, -67.49999999999997158 ) ) ;
#3263 = VECTOR ( 'NONE', #15575, 1000.000000000000000 ) ;
#3264 = DIRECTION ( 'NONE',  ( -0.000000000000000000, -0.000000000000000000, -1.000000000000000000 ) ) ;
#3265 = DIRECTION ( 'NONE',  ( 1.000000000000000000, 0.000000000000000000, 0.000000000000000000 ) ) ;
#3266 = DIRECTION ( 'NONE',  ( 0.4338837391175654479, -0.9009688679024155933, 0.000000000000000000 ) ) ;
#3267 = FACE_OUTER_BOUND ( 'NONE', #1604, .T. ) ;
#3268 = ORIENTED_EDGE ( 'NONE', *, *, #11842, .F. ) ;
#3269 = FACE_OUTER_BOUND ( 'NONE', #11103, .T. ) ;
#3270 = ORIENTED_EDGE ( 'NONE', *, *, #13126, .F. ) ;
#3271 = EDGE_CURVE ( 'NONE', #573, #15878, #18059, .T. ) ;
#3272 = EDGE_CURVE ( 'NONE', #8591, #18684, #15440, .T. ) ;
#3273 = ORIENTED_EDGE ( 'NONE', *, *, #6591, .T. ) ;
#3274 = EDGE_CURVE ( 'NONE', #9040, #13775, #11187, .T. ) ;
#3275 = PRODUCT_DEFINITION ( 'UNKNOWN', '', #10143, #7010 ) ;
#3276 = FACE_OUTER_BOUND ( 'NONE', #2176, .T. ) ;
#3277 = ORIENTED_EDGE ( 'NONE', *, *, #6383, .F. ) ;
#3278 = DIRECTION ( 'NONE',  ( 1.000000000000000000, 0.000000000000000000, -6.994638739193269649E-15 ) ) ;
#3279 = CYLINDRICAL_SURFACE ( 'NONE', #10565, 7.500000000000007105 ) ;
#3280 = EDGE_LOOP ( 'NONE', ( #17138, #15660, #19587 ) ) ;
#3281 = CARTESIAN_POINT ( 'NONE',  ( 0.5590800469813620444, -9.968355046870076563, -0.7343025909353907421 ) ) ;
#3282 = CARTESIAN_POINT ( 'NONE',  ( 60.00000000000000711, 6.284666409917639535E-13, -105.0000000000000142 ) ) ;
#3283 = EDGE_CURVE ( 'NONE', #10155, #10316, #18530, .T. ) ;
#3284 = DIRECTION ( 'NONE',  ( 6.982962677686266711E-15, -0.000000000000000000, 1.000000000000000000 ) ) ;
#3285 = AXIS2_PLACEMENT_3D ( 'NONE', #3463, #5108, #15847 ) ;
#3286 = DIRECTION ( 'NONE',  ( -6.982962677686266711E-15, 0.000000000000000000, -1.000000000000000000 ) ) ;
#3287 = ORIENTED_EDGE ( 'NONE', *, *, #9603, .F. ) ;
#3288 = CARTESIAN_POINT ( 'NONE',  ( -53.86996498385652643, -28.06584155524119595, 283.5832628385307999 ) ) ;
#3289 = PRODUCT_DEFINITION_FORMATION_WITH_SPECIFIED_SOURCE ( 'ANY', '', #1474, .NOT_KNOWN. ) ;
#3290 = DIRECTION ( 'NONE',  ( 0.000000000000000000, 0.000000000000000000, 1.000000000000000000 ) ) ;
#3291 = CYLINDRICAL_SURFACE ( 'NONE', #13183, 106.4288957539801004 ) ;
#3292 = VECTOR ( 'NONE', #2804, 1000.000000000000000 ) ;
#3293 = CARTESIAN_POINT ( 'NONE',  ( 82.18957362173902936, -125.4791168306830258, 32.98504099366878961 ) ) ;
#3294 = ORIENTED_EDGE ( 'NONE', *, *, #121, .T. ) ;
#3295 = FACE_OUTER_BOUND ( 'NONE', #6584, .T. ) ;
#3296 = DIRECTION ( 'NONE',  ( -0.9848077530122066880, -0.1736481776669374366, 0.000000000000000000 ) ) ;
#3297 = EDGE_CURVE ( 'NONE', #7092, #6348, #9320, .T. ) ;
#3298 = EDGE_CURVE ( 'NONE', #18469, #1479, #8572, .T. ) ;
#3299 = ORIENTED_EDGE ( 'NONE', *, *, #8527, .T. ) ;
#3300 = VERTEX_POINT ( 'NONE', #1446 ) ;
#3301 = VERTEX_POINT ( 'NONE', #4511 ) ;
#3302 = EDGE_LOOP ( 'NONE', ( #5917, #12026 ) ) ;
#3303 = ADVANCED_FACE ( 'NONE', ( #12276, #7677 ), #20161, .F. ) ;
#3304 = DIRECTION ( 'NONE',  ( -0.9749279121818257288, 0.2225209339563050392, 0.000000000000000000 ) ) ;
#3305 = AXIS2_PLACEMENT_3D ( 'NONE', #11624, #17881, #7320 ) ;
#3306 = PLANE ( 'NONE',  #5780 ) ;
#3307 = ORIENTED_EDGE ( 'NONE', *, *, #18772, .T. ) ;
#3308 = CIRCLE ( 'NONE', #19312, 150.0000000000000284 ) ;
#3309 = DIRECTION ( 'NONE',  ( -0.000000000000000000, -0.000000000000000000, 1.000000000000000000 ) ) ;
#3310 = LINE ( 'NONE', #18968, #17848 ) ;
#3311 = CARTESIAN_POINT ( 'NONE',  ( -87.34436178610755519, -121.9468435064291612, 43.95302374537314449 ) ) ;
#3312 = DIRECTION ( 'NONE',  ( 1.000000000000000000, 0.000000000000000000, -6.976128451377902853E-15 ) ) ;
#3313 = CARTESIAN_POINT ( 'NONE',  ( -119.1059459284890778, 73.60494313202988792, 38.81136714554597233 ) ) ;
#3314 = DIRECTION ( 'NONE',  ( -0.1736481776669340227, 0.9848077530122073542, 0.000000000000000000 ) ) ;
#3315 = PLANE ( 'NONE',  #8877 ) ;
#3316 = CARTESIAN_POINT ( 'NONE',  ( 159.9599531637113330, -36.50981547336952104, 60.00000000000000000 ) ) ;
#3317 = DIRECTION ( 'NONE',  ( 6.982962677686266711E-15, -0.000000000000000000, 1.000000000000000000 ) ) ;
#3318 = CARTESIAN_POINT ( 'NONE',  ( -134.1895921339651920, -76.75826352743507641, 35.74347206174024905 ) ) ;
#3319 = ORIENTED_EDGE ( 'NONE', *, *, #2589, .F. ) ;
#3320 = VECTOR ( 'NONE', #3679, 1000.000000000000000 ) ;
#3321 = CARTESIAN_POINT ( 'NONE',  ( -78.26059000578311498, 0.8220851292432594937, 112.7772637782949516 ) ) ;
#3322 = AXIS2_PLACEMENT_3D ( 'NONE', #13528, #18053, #16618 ) ;
#3323 = ORIENTED_EDGE ( 'NONE', *, *, #3755, .F. ) ;
#3324 = ORIENTED_EDGE ( 'NONE', *, *, #3886, .T. ) ;
#3325 = ORIENTED_EDGE ( 'NONE', *, *, #287, .F. ) ;
#3326 = CARTESIAN_POINT ( 'NONE',  ( -144.8005054862046848, -14.35567093075204248, 8.862053436824973929 ) ) ;
#3327 = DIRECTION ( 'NONE',  ( -0.7818314824680222541, -0.6234898018587428092, 0.000000000000000000 ) ) ;
#3328 = LINE ( 'NONE', #53, #15952 ) ;
#3329 = CARTESIAN_POINT ( 'NONE',  ( 0.000000000000000000, 0.000000000000000000, 283.5832628385307999 ) ) ;
#3330 = CARTESIAN_POINT ( 'NONE',  ( 71.18887634719571622, -147.8252249328912740, 60.00000000000000000 ) ) ;
#3331 = CARTESIAN_POINT ( 'NONE',  ( 76.92888220842486646, -14.39940464655733976, 112.0427633081292385 ) ) ;
#3332 = CARTESIAN_POINT ( 'NONE',  ( 118.3534152657848608, 114.7431683447366595, 39.99999999999999289 ) ) ;
#3333 = CARTESIAN_POINT ( 'NONE',  ( 98.69444885161529157, -132.3639744934813507, 34.75573401544776431 ) ) ;
#3334 = FACE_OUTER_BOUND ( 'NONE', #5200, .T. ) ;
#3335 = VERTEX_POINT ( 'NONE', #1342 ) ;
#3336 = CARTESIAN_POINT ( 'NONE',  ( 134.4925794577852685, -74.66012650511407855, 33.94317531104282892 ) ) ;
#3337 = PLANE ( 'NONE',  #9029 ) ;
#3338 = ORIENTED_EDGE ( 'NONE', *, *, #18363, .T. ) ;
#3339 = ORIENTED_EDGE ( 'NONE', *, *, #9551, .F. ) ;
#3340 = ORIENTED_EDGE ( 'NONE', *, *, #19364, .F. ) ;
#3341 = EDGE_LOOP ( 'NONE', ( #9492, #4784, #5801, #2110, #12859, #14208, #1735, #19633, #12646, #958, #17042, #11082, #11220, #15387, #15418, #2422, #7191, #11685, #1581, #3959, #19178, #18458, #2245, #18129, #7799, #17297, #2967 ) ) ;
#3342 = ADVANCED_FACE ( 'NONE', ( #1549 ), #13916, .F. ) ;
#3343 = DIRECTION ( 'NONE',  ( 0.9848077530122074652, 0.1736481776669340504, 0.000000000000000000 ) ) ;
#3344 = AXIS2_PLACEMENT_3D ( 'NONE', #7704, #16924, #12304 ) ;
#3345 = VECTOR ( 'NONE', #16519, 1000.000000000000000 ) ;
#3346 = VERTEX_POINT ( 'NONE', #1131 ) ;
#3347 = CARTESIAN_POINT ( 'NONE',  ( 4.581103194070568208, -3.453261854573344447, 283.5832628385307999 ) ) ;
#3348 = CARTESIAN_POINT ( 'NONE',  ( -104.1558342746901218, -124.2522228486704421, 39.43806085740693135 ) ) ;
#3349 = CARTESIAN_POINT ( 'NONE',  ( 0.000000000000000000, 0.000000000000000000, 132.4711112102474146 ) ) ;
#3350 = ORIENTED_EDGE ( 'NONE', *, *, #18427, .T. ) ;
#3351 = AXIS2_PLACEMENT_3D ( 'NONE', #11937, #14923, #910 ) ;
#3352 = DIRECTION ( 'NONE',  ( 0.000000000000000000, 0.000000000000000000, 1.000000000000000000 ) ) ;
#3353 = CARTESIAN_POINT ( 'NONE',  ( 0.3563104543936346236, 6.049278984716044860, 7.522341449313135975 ) ) ;
#3354 = ORIENTED_EDGE ( 'NONE', *, *, #14924, .F. ) ;
#3355 = ADVANCED_FACE ( 'NONE', ( #12381 ), #5854, .T. ) ;
#3356 = DIRECTION ( 'NONE',  ( 0.000000000000000000, 0.000000000000000000, 1.000000000000000000 ) ) ;
#3357 = CARTESIAN_POINT ( 'NONE',  ( 61.81362617575101837, -11.73417718768070550, 132.4711112102474146 ) ) ;
#3358 = EDGE_CURVE ( 'NONE', #7769, #14586, #4617, .T. ) ;
#3359 = ADVANCED_FACE ( 'NONE', ( #4204 ), #7371, .F. ) ;
#3360 = FACE_OUTER_BOUND ( 'NONE', #14735, .T. ) ;
#3361 = AXIS2_PLACEMENT_3D ( 'NONE', #16481, #2268, #14733 ) ;
#3362 = AXIS2_PLACEMENT_3D ( 'NONE', #10149, #5644, #8610 ) ;
#3363 = DIRECTION ( 'NONE',  ( 0.000000000000000000, 0.000000000000000000, -1.000000000000000000 ) ) ;
#3364 = LINE ( 'NONE', #8060, #13066 ) ;
#3365 = CARTESIAN_POINT ( 'NONE',  ( -75.16204133714633429, 118.1133591082685683, 1.232491660827630842 ) ) ;
#3366 = VERTEX_POINT ( 'NONE', #12064 ) ;
#3367 = CARTESIAN_POINT ( 'NONE',  ( 77.21438937758502163, 12.78021302872874010, 248.9926560891072143 ) ) ;
#3368 = ORIENTED_EDGE ( 'NONE', *, *, #12134, .T. ) ;
#3369 = AXIS2_PLACEMENT_3D ( 'NONE', #8959, #1301, #5805 ) ;
#3370 = ORIENTED_EDGE ( 'NONE', *, *, #11115, .F. ) ;
#3371 = ADVANCED_FACE ( 'NONE', ( #2783 ), #18328, .F. ) ;
#3372 = CARTESIAN_POINT ( 'NONE',  ( 97.50000000000002842, -199.9999999999999716, 40.00000000000000000 ) ) ;
#3373 = ORIENTED_EDGE ( 'NONE', *, *, #157, .T. ) ;
#3374 = CARTESIAN_POINT ( 'NONE',  ( 2.629250726500717672, 60.68567895461850270, 283.5832628385307999 ) ) ;
#3375 = CARTESIAN_POINT ( 'NONE',  ( -5.524863963826822655, -116.0870680293436408, 14.88498244535549020 ) ) ;
#3376 = CIRCLE ( 'NONE', #17452, 7.500000000000020428 ) ;
#3377 = ORIENTED_EDGE ( 'NONE', *, *, #4414, .F. ) ;
#3378 = VECTOR ( 'NONE', #7689, 1000.000000000000000 ) ;
#3379 = CARTESIAN_POINT ( 'NONE',  ( -47.66508197439443961, 41.06890862491521688, 293.5832628385307999 ) ) ;
#3380 = CYLINDRICAL_SURFACE ( 'NONE', #6596, 10.00000000000000888 ) ;
#3381 = EDGE_CURVE ( 'NONE', #1807, #11267, #9004, .T. ) ;
#3382 = EDGE_CURVE ( 'NONE', #8156, #7092, #1233, .T. ) ;
#3383 = AXIS2_PLACEMENT_3D ( 'NONE', #749, #2199, #19286 ) ;
#3384 = EDGE_CURVE ( 'NONE', #13329, #16043, #4409, .T. ) ;
#3385 = FACE_OUTER_BOUND ( 'NONE', #17886, .T. ) ;
#3386 = DIRECTION ( 'NONE',  ( 1.000000000000000000, 0.000000000000000000, 0.000000000000000000 ) ) ;
#3387 = ORIENTED_EDGE ( 'NONE', *, *, #18913, .T. ) ;
#3388 = CARTESIAN_POINT ( 'NONE',  ( -59.58067424803613221, 20.21777810286735999, 132.4711112102474146 ) ) ;
#3389 = VECTOR ( 'NONE', #2870, 1000.000000000000000 ) ;
#3390 = DIRECTION ( 'NONE',  ( 1.000000000000000000, 0.000000000000000000, 0.000000000000000000 ) ) ;
#3391 = DIRECTION ( 'NONE',  ( 0.000000000000000000, 0.000000000000000000, 1.000000000000000000 ) ) ;
#3392 = CARTESIAN_POINT ( 'NONE',  ( 98.69108797088914287, -112.9688971639519934, 49.90760263315277712 ) ) ;
#3393 = EDGE_LOOP ( 'NONE', ( #12182, #17918, #10781 ) ) ;
#3394 =( BOUNDED_SURFACE ( )  B_SPLINE_SURFACE ( 3, 2, ( 
 ( #4296, #19743, #10139 ),
 ( #5440, #5636, #16489 ),
 ( #4091, #5740, #14934 ),
 ( #923, #7179, #11761 ),
 ( #16684, #18212, #16782 ),
 ( #19547, #7364, #13595 ),
 ( #2671, #727, #2566 ),
 ( #8800, #7075, #13393 ),
 ( #15042, #14746, #11667 ),
 ( #16391, #17928, #5540 ),
 ( #19840, #12057, #18320 ),
 ( #10523, #13289, #8506 ),
 ( #3900, #2370, #8604 ),
 ( #14839, #824, #16882 ),
 ( #10626, #14114, #102 ),
 ( #4607, #9098, #7462 ),
 ( #2973, #4713, #9311 ),
 ( #14011, #18631, #20152 ),
 ( #15661, #15237, #18836 ),
 ( #18424, #15340, #4399 ),
 ( #10733, #12369, #18521 ),
 ( #2872, #3180, #20051 ),
 ( #19944, #1332, #9203 ),
 ( #6353, #10830, #1540 ),
 ( #17089, #7564, #9413 ),
 ( #13806, #10938, #15554 ),
 ( #6256, #12572, #4501 ),
 ( #13702, #4821, #2 ),
 ( #6049, #12269, #16988 ),
 ( #7871, #18731, #15449 ),
 ( #3078, #1438, #1645 ),
 ( #7669, #1224, #11041 ) ),
 .UNSPECIFIED., .F., .F., .F. ) 
 B_SPLINE_SURFACE_WITH_KNOTS ( ( 4, 2, 2, 2, 2, 2, 2, 2, 2, 2, 2, 2, 2, 2, 2, 4 ),
 ( 3, 3 ),
 ( 0.02531008572351750585, 0.02976618726483498678, 0.03422228880615246771, 0.03645033957681120818, 0.03867839034746994864, 0.04313449188878743651, 0.04424851727411681368, 0.04536254265944618391, 0.04759059343010492438, 0.04981864420076366484, 0.05093266958609303507, 0.05204669497142240531, 0.05650279651273988624, 0.05761682189806925647, 0.05873084728339862670, 0.06095889805405736717 ),
 ( 0.000000000000000000, 1.000000000000000000 ),
 .UNSPECIFIED. ) 
 GEOMETRIC_REPRESENTATION_ITEM ( )  RATIONAL_B_SPLINE_SURFACE ( (
 ( 1.000000000000000000, 0.7071067811865475727, 1.000000000000000000),
 ( 1.000000000000000000, 0.6938858163890799791, 1.000000000000000000),
 ( 1.000000000000000000, 0.6806631602001719239, 1.000000000000000000),
 ( 1.000000000000000000, 0.6542661407885864699, 1.000000000000000000),
 ( 1.000000000000000000, 0.6410910482669636146, 1.000000000000000000),
 ( 1.000000000000000000, 0.6214215355382751715, 1.000000000000000000),
 ( 1.000000000000000000, 0.6148567640637033760, 1.000000000000000000),
 ( 1.000000000000000000, 0.6019746658714538734, 1.000000000000000000),
 ( 1.000000000000000000, 0.5956402134851142005, 1.000000000000000000),
 ( 1.000000000000000000, 0.5769855966611233677, 1.000000000000000000),
 ( 1.000000000000000000, 0.5650096313354644462, 1.000000000000000000),
 ( 1.000000000000000000, 0.5507648555196259510, 1.000000000000000000),
 ( 1.000000000000000000, 0.5479490128870576626, 1.000000000000000000),
 ( 1.000000000000000000, 0.5424554856653802659, 1.000000000000000000),
 ( 1.000000000000000000, 0.5397704441656565599, 1.000000000000000000),
 ( 1.000000000000000000, 0.5319045985432593326, 1.000000000000000000),
 ( 1.000000000000000000, 0.5269125948470546605, 1.000000000000000000),
 ( 1.000000000000000000, 0.5174644824775621599, 1.000000000000000000),
 ( 1.000000000000000000, 0.5130081457584921845, 1.000000000000000000),
 ( 1.000000000000000000, 0.5067628861632251791, 1.000000000000000000),
 ( 1.000000000000000000, 0.5047490957320777127, 1.000000000000000000),
 ( 1.000000000000000000, 0.5009263418717799787, 1.000000000000000000),
 ( 1.000000000000000000, 0.4991119735066631979, 1.000000000000000000),
 ( 1.000000000000000000, 0.4905251103114823819, 1.000000000000000000),
 ( 1.000000000000000000, 0.4851887169567591918, 1.000000000000000000),
 ( 1.000000000000000000, 0.4806071066594930219, 1.000000000000000000),
 ( 1.000000000000000000, 0.4797938356041033248, 1.000000000000000000),
 ( 1.000000000000000000, 0.4784048377102336214, 1.000000000000000000),
 ( 1.000000000000000000, 0.4778282137467559920, 1.000000000000000000),
 ( 1.000000000000000000, 0.4764456491719189501, 1.000000000000000000),
 ( 1.000000000000000000, 0.4759864261384231243, 1.000000000000000000),
 ( 1.000000000000000000, 0.4759858191164941243, 1.000000000000000000) ) ) 
 REPRESENTATION_ITEM ( '' )  SURFACE ( )  );
#3395 = CARTESIAN_POINT ( 'NONE',  ( 15.91767397667354800, 164.0736214083062805, 39.99999999999999289 ) ) ;
#3396 = CARTESIAN_POINT ( 'NONE',  ( -104.9326538737192323, 107.1912678330463677, 44.68324212414002261 ) ) ;
#3397 = AXIS2_PLACEMENT_3D ( 'NONE', #17888, #3862, #10107 ) ;
#3398 = ORIENTED_EDGE ( 'NONE', *, *, #20167, .T. ) ;
#3399 = EDGE_LOOP ( 'NONE', ( #2716, #2111, #12208, #14666 ) ) ;
#3400 = ORIENTED_EDGE ( 'NONE', *, *, #6622, .T. ) ;
#3401 = EDGE_CURVE ( 'NONE', #17191, #3695, #12037, .T. ) ;
#3402 = SHAPE_DEFINITION_REPRESENTATION ( #12918, #2084 ) ;
#3403 = CIRCLE ( 'NONE', #7613, 5.035999999999999588 ) ;
#3404 = ORIENTED_EDGE ( 'NONE', *, *, #18225, .T. ) ;
#3405 = DIRECTION ( 'NONE',  ( 1.000000000000000000, 0.000000000000000000, 0.000000000000000000 ) ) ;
#3406 = CARTESIAN_POINT ( 'NONE',  ( -121.0878816972190322, 88.53962377493060387, 43.43999758500223862 ) ) ;
#3407 = VECTOR ( 'NONE', #8574, 1000.000000000000000 ) ;
#3408 = VERTEX_POINT ( 'NONE', #1749 ) ;
#3409 = CARTESIAN_POINT ( 'NONE',  ( -37.09555676056967144, 45.48770046196298011, 132.4711112102474146 ) ) ;
#3410 = CARTESIAN_POINT ( 'NONE',  ( 133.7387326730402322, -67.93012127445985016, 39.56577003862501840 ) ) ;
#3411 = EDGE_CURVE ( 'NONE', #12392, #19032, #9419, .T. ) ;
#3412 = EDGE_CURVE ( 'NONE', #13701, #5147, #9425, .T. ) ;
#3413 = EDGE_CURVE ( 'NONE', #13701, #11033, #4863, .T. ) ;
#3414 = CARTESIAN_POINT ( 'NONE',  ( -122.5787829483134601, 67.64166609452395562, 37.66536492912700851 ) ) ;
#3415 = CARTESIAN_POINT ( 'NONE',  ( -7.499999999999583444, -60.00000000000000000, -115.0000000000000000 ) ) ;
#3416 = VECTOR ( 'NONE', #3314, 1000.000000000000114 ) ;
#3417 = CARTESIAN_POINT ( 'NONE',  ( -12.78021302872797449, 77.21438937758516374, 112.0427633081291816 ) ) ;
#3418 = DIRECTION ( 'NONE',  ( -0.000000000000000000, -0.000000000000000000, 1.000000000000000000 ) ) ;
#3419 = DIRECTION ( 'NONE',  ( 0.000000000000000000, 0.000000000000000000, -1.000000000000000000 ) ) ;
#3420 = ORIENTED_EDGE ( 'NONE', *, *, #8373, .T. ) ;
#3421 = DIRECTION ( 'NONE',  ( 1.000000000000000000, 0.000000000000000000, 0.000000000000000000 ) ) ;
#3422 =( GEOMETRIC_REPRESENTATION_CONTEXT ( 3 ) GLOBAL_UNCERTAINTY_ASSIGNED_CONTEXT ( ( #12118 ) ) GLOBAL_UNIT_ASSIGNED_CONTEXT ( ( #18810, #17376, #7944 ) ) REPRESENTATION_CONTEXT ( 'NONE', 'WORKASPACE' ) );
#3423 = ADVANCED_FACE ( 'NONE', ( #111 ), #3291, .F. ) ;
#3424 = VERTEX_POINT ( 'NONE', #11256 ) ;
#3425 = EDGE_LOOP ( 'NONE', ( #16382, #14638, #12899, #18330 ) ) ;
#3426 = ORIENTED_EDGE ( 'NONE', *, *, #8420, .F. ) ;
#3427 = LINE ( 'NONE', #1892, #10264 ) ;
#3428 = DIRECTION ( 'NONE',  ( -1.000000000000000000, 0.000000000000000000, 0.000000000000000000 ) ) ;
#3429 = CARTESIAN_POINT ( 'NONE',  ( -59.51523122377251696, 12.14914984460740754, 283.5832628385307999 ) ) ;
#3430 = ORIENTED_EDGE ( 'NONE', *, *, #4220, .T. ) ;
#3431 = FACE_OUTER_BOUND ( 'NONE', #19180, .T. ) ;
#3432 = LINE ( 'NONE', #14578, #18368 ) ;
#3433 = CARTESIAN_POINT ( 'NONE',  ( 0.000000000000000000, 164.0736214083062805, 39.99999999999999289 ) ) ;
#3434 = CARTESIAN_POINT ( 'NONE',  ( 98.02151343901461189, -133.2674925500989218, 33.21951988572780579 ) ) ;
#3435 = AXIS2_PLACEMENT_3D ( 'NONE', #5026, #4929, #14326 ) ;
#3436 = CARTESIAN_POINT ( 'NONE',  ( -28.94886449118903826, 53.40063514825088475, 283.5832628385307999 ) ) ;
#3437 = ADVANCED_FACE ( 'NONE', ( #7882 ), #10947, .T. ) ;
#3438 = ORIENTED_EDGE ( 'NONE', *, *, #3401, .T. ) ;
#3439 = CARTESIAN_POINT ( 'NONE',  ( -60.47951622432784546, -49.67518383744813804, 132.4711112102474146 ) ) ;
#3440 = AXIS2_PLACEMENT_3D ( 'NONE', #10713, #1315, #12142 ) ;
#3441 = CARTESIAN_POINT ( 'NONE',  ( 134.5752827950141750, -74.04736996659980264, 33.19974057736502004 ) ) ;
#3442 = ORIENTED_EDGE ( 'NONE', *, *, #6538, .F. ) ;
#3443 = ORIENTED_EDGE ( 'NONE', *, *, #8164, .T. ) ;
#3444 = VERTEX_POINT ( 'NONE', #4937 ) ;
#3445 = ORIENTED_EDGE ( 'NONE', *, *, #16774, .F. ) ;
#3446 = CARTESIAN_POINT ( 'NONE',  ( -77.21438937758510690, -12.78021302872823384, 112.0427633081291816 ) ) ;
#3447 = VERTEX_POINT ( 'NONE', #418 ) ;
#3448 = CARTESIAN_POINT ( 'NONE',  ( 28.63313560863472063, -51.23821591265105013, 248.9926560891072143 ) ) ;
#3449 = AXIS2_PLACEMENT_3D ( 'NONE', #8700, #11952, #5838 ) ;
#3450 = DIRECTION ( 'NONE',  ( -0.4338837391175549008, -0.9009688679024205893, 0.000000000000000000 ) ) ;
#3451 = CARTESIAN_POINT ( 'NONE',  ( -97.49999999999998579, -133.9542832461881687, 10.00000000000000178 ) ) ;
#3452 = DIRECTION ( 'NONE',  ( 0.000000000000000000, 0.000000000000000000, 1.000000000000000000 ) ) ;
#3453 = EDGE_LOOP ( 'NONE', ( #11712, #4339, #4209, #20136 ) ) ;
#3454 = CARTESIAN_POINT ( 'NONE',  ( 131.9327818480801682, -71.37991627326495347, -3.783672495338017860 ) ) ;
#3455 = DIRECTION ( 'NONE',  ( -0.8479630283625716469, 0.5300553768524345344, 0.000000000000000000 ) ) ;
#3456 = ORIENTED_EDGE ( 'NONE', *, *, #3471, .T. ) ;
#3457 = CARTESIAN_POINT ( 'NONE',  ( 0.000000000000000000, 164.0736214083062805, 60.00000000000000000 ) ) ;
#3458 = LINE ( 'NONE', #2032, #2273 ) ;
#3459 = CIRCLE ( 'NONE', #13569, 112.8770930172170210 ) ;
#3460 = EDGE_CURVE ( 'NONE', #720, #19683, #19414, .T. ) ;
#3461 = FACE_OUTER_BOUND ( 'NONE', #9802, .T. ) ;
#3462 = DIRECTION ( 'NONE',  ( 1.000000000000000000, 0.000000000000000000, 0.000000000000000000 ) ) ;
#3463 = CARTESIAN_POINT ( 'NONE',  ( 0.000000000000000000, 0.000000000000000000, 283.5832628385307999 ) ) ;
#3464 = CIRCLE ( 'NONE', #14881, 10.00000000000000888 ) ;
#3465 = CARTESIAN_POINT ( 'NONE',  ( 86.48208760716208587, -122.5631135004755805, 43.00921107642988517 ) ) ;
#3466 = ORIENTED_EDGE ( 'NONE', *, *, #9851, .F. ) ;
#3467 = DIRECTION ( 'NONE',  ( -0.000000000000000000, -0.000000000000000000, 1.000000000000000000 ) ) ;
#3468 = ORIENTED_EDGE ( 'NONE', *, *, #8639, .F. ) ;
#3469 = ORIENTED_EDGE ( 'NONE', *, *, #15106, .F. ) ;
#3470 = FACE_OUTER_BOUND ( 'NONE', #6199, .T. ) ;
#3471 = EDGE_CURVE ( 'NONE', #10476, #12392, #14336, .T. ) ;
#3472 = ORIENTED_EDGE ( 'NONE', *, *, #360, .F. ) ;
#3473 = VECTOR ( 'NONE', #17804, 1000.000000000000114 ) ;
#3474 = CARTESIAN_POINT ( 'NONE',  ( 25.98398601615845038, 7.853099154550832850, 39.88498244535526993 ) ) ;
#3475 = AXIS2_PLACEMENT_3D ( 'NONE', #14393, #4992, #17061 ) ;
#3476 = PLANE ( 'NONE',  #18757 ) ;
#3477 = ORIENTED_EDGE ( 'NONE', *, *, #14791, .T. ) ;
#3478 = CARTESIAN_POINT ( 'NONE',  ( -110.0000000000000142, 285.0000000000000568, 5.000000000000000888 ) ) ;
#3479 = CARTESIAN_POINT ( 'NONE',  ( -110.0000000000000142, 275.0000000000000000, -75.00000000000000000 ) ) ;
#3480 = AXIS2_PLACEMENT_3D ( 'NONE', #4157, #16644, #16452 ) ;
#3481 = DIRECTION ( 'NONE',  ( 1.000000000000000000, 0.000000000000000000, 0.000000000000000000 ) ) ;
#3482 = ADVANCED_FACE ( 'NONE', ( #313 ), #3592, .T. ) ;
#3483 = LINE ( 'NONE', #1544, #16344 ) ;
#3484 = LINE ( 'NONE', #2059, #16809 ) ;
#3485 = VERTEX_POINT ( 'NONE', #18844 ) ;
#3486 = DIRECTION ( 'NONE',  ( 1.000000000000000000, 0.000000000000000000, 0.000000000000000000 ) ) ;
#3487 = DIRECTION ( 'NONE',  ( 0.000000000000000000, 0.000000000000000000, 1.000000000000000000 ) ) ;
#3488 = CARTESIAN_POINT ( 'NONE',  ( -1.396592535537253342E-14, 0.000000000000000000, 39.88498244535545467 ) ) ;
#3489 = LINE ( 'NONE', #14534, #9228 ) ;
#3490 = AXIS2_PLACEMENT_3D ( 'NONE', #3457, #15736, #19021 ) ;
#3491 = ORIENTED_EDGE ( 'NONE', *, *, #17032, .T. ) ;
#3492 = VECTOR ( 'NONE', #13412, 1000.000000000000000 ) ;
#3493 = DIRECTION ( 'NONE',  ( -1.000000000000000000, 4.650550193362991910E-16, 0.000000000000000000 ) ) ;
#3494 = CARTESIAN_POINT ( 'NONE',  ( 50.37374754117451658, -141.2886604036503115, 49.99999999999999289 ) ) ;
#3495 = VERTEX_POINT ( 'NONE', #4828 ) ;
#3496 = VERTEX_POINT ( 'NONE', #11051 ) ;
#3497 = ORIENTED_EDGE ( 'NONE', *, *, #5179, .F. ) ;
#3498 = EDGE_CURVE ( 'NONE', #14660, #18649, #16015, .T. ) ;
#3499 = ORIENTED_EDGE ( 'NONE', *, *, #960, .F. ) ;
#3500 = EDGE_CURVE ( 'NONE', #4491, #18721, #7194, .T. ) ;
#3501 = DIRECTION ( 'NONE',  ( 0.000000000000000000, 0.000000000000000000, 1.000000000000000000 ) ) ;
#3502 = ORIENTED_EDGE ( 'NONE', *, *, #9739, .F. ) ;
#3503 = FACE_OUTER_BOUND ( 'NONE', #7245, .T. ) ;
#3504 = DIRECTION ( 'NONE',  ( 0.4999999999999925060, -0.8660254037844429265, -4.304393070272789636E-15 ) ) ;
#3505 = FACE_OUTER_BOUND ( 'NONE', #15361, .T. ) ;
#3506 = LINE ( 'NONE', #12910, #15 ) ;
#3507 =( BOUNDED_CURVE ( )  B_SPLINE_CURVE ( 3, ( #10898, #12019, #165, #12639 ),
 .UNSPECIFIED., .F., .F. ) 
 B_SPLINE_CURVE_WITH_KNOTS ( ( 4, 4 ),
 ( 0.000000000000000000, 1.570796326794896558 ),
 .UNSPECIFIED. ) 
 CURVE ( )  GEOMETRIC_REPRESENTATION_ITEM ( )  RATIONAL_B_SPLINE_CURVE ( ( 1.000000000000000000, 0.8047378541243649375, 0.8047378541243649375, 1.000000000000000000 ) ) 
 REPRESENTATION_ITEM ( '' )  );
#3508 = DIRECTION ( 'NONE',  ( -0.8660254037844432595, 0.4999999999999919509, 0.000000000000000000 ) ) ;
#3509 = VECTOR ( 'NONE', #2855, 1000.000000000000000 ) ;
#3510 = EDGE_CURVE ( 'NONE', #13184, #15860, #14228, .T. ) ;
#3511 = DIRECTION ( 'NONE',  ( 0.7660444431189813441, -0.6427876096865353661, 0.000000000000000000 ) ) ;
#3512 = AXIS2_PLACEMENT_3D ( 'NONE', #1575, #3114, #10772 ) ;
#3513 = DIRECTION ( 'NONE',  ( -0.9009688679024155933, -0.4338837391175654479, 0.000000000000000000 ) ) ;
#3514 = CARTESIAN_POINT ( 'NONE',  ( -56.50138340076688337, 22.29928840491054132, 283.5832628385307999 ) ) ;
#3515 = DIRECTION ( 'NONE',  ( 0.4338837391175662250, -0.9009688679024151492, 0.000000000000000000 ) ) ;
#3516 = EDGE_LOOP ( 'NONE', ( #12107, #19283, #9218, #5758 ) ) ;
#3517 = LINE ( 'NONE', #243, #19676 ) ;
#3518 = ORIENTED_EDGE ( 'NONE', *, *, #13615, .F. ) ;
#3519 = EDGE_CURVE ( 'NONE', #19407, #20158, #15767, .T. ) ;
#3520 = AXIS2_PLACEMENT_3D ( 'NONE', #9178, #13881, #4170 ) ;
#3521 = ADVANCED_FACE ( 'NONE', ( #14532 ), #8188, .F. ) ;
#3522 = ORIENTED_EDGE ( 'NONE', *, *, #5242, .F. ) ;
#3523 = EDGE_CURVE ( 'NONE', #15303, #3260, #19297, .T. ) ;
#3524 = PRODUCT_DEFINITION ( 'UNKNOWN', '', #671, #668 ) ;
#3525 = VECTOR ( 'NONE', #17883, 1000.000000000000000 ) ;
#3526 = VECTOR ( 'NONE', #16223, 1000.000000000000000 ) ;
#3527 = EDGE_LOOP ( 'NONE', ( #8493, #14502, #18442, #6426 ) ) ;
#3528 = CARTESIAN_POINT ( 'NONE',  ( 51.77076963420847733, -31.77187437101486367, 293.5832628385307999 ) ) ;
#3529 = CARTESIAN_POINT ( 'NONE',  ( 58.69016442926523069, -0.8220851292429179891, 248.9926560891072143 ) ) ;
#3530 = DIRECTION ( 'NONE',  ( -0.000000000000000000, -0.000000000000000000, 1.000000000000000000 ) ) ;
#3531 = CARTESIAN_POINT ( 'NONE',  ( -134.7652707650784407, -31.41120252075685215, -19.73219286542039441 ) ) ;
#3532 = CARTESIAN_POINT ( 'NONE',  ( -110.0000000000000142, 285.0000000000000568, -67.49999999999997158 ) ) ;
#3533 = EDGE_CURVE ( 'NONE', #8624, #10590, #5136, .T. ) ;
#3534 = EDGE_CURVE ( 'NONE', #20066, #7454, #8288, .T. ) ;
#3535 = DIRECTION ( 'NONE',  ( -0.000000000000000000, -0.000000000000000000, 1.000000000000000000 ) ) ;
#3536 = CARTESIAN_POINT ( 'NONE',  ( 7.948937137877743808, -60.22232964560488000, 293.5832628385307999 ) ) ;
#3537 = DIRECTION ( 'NONE',  ( 0.000000000000000000, 0.5000000000000018874, 0.8660254037844374864 ) ) ;
#3538 = LINE ( 'NONE', #14382, #6471 ) ;
#3539 = VECTOR ( 'NONE', #3530, 1000.000000000000000 ) ;
#3540 = ORIENTED_EDGE ( 'NONE', *, *, #19008, .F. ) ;
#3541 = VECTOR ( 'NONE', #5142, 1000.000000000000000 ) ;
#3542 = CARTESIAN_POINT ( 'NONE',  ( -59.06449708980197499, -51.36153797460887915, 110.7293897666001214 ) ) ;
#3543 = ORIENTED_EDGE ( 'NONE', *, *, #9643, .T. ) ;
#3544 = ORIENTED_EDGE ( 'NONE', *, *, #12605, .T. ) ;
#3545 = VERTEX_POINT ( 'NONE', #19249 ) ;
#3546 = ADVANCED_FACE ( 'NONE', ( #2453 ), #11746, .F. ) ;
#3547 = ORIENTED_EDGE ( 'NONE', *, *, #1891, .T. ) ;
#3548 = CIRCLE ( 'NONE', #14966, 3.224098631618461219 ) ;
#3549 = VERTEX_POINT ( 'NONE', #2264 ) ;
#3550 = CARTESIAN_POINT ( 'NONE',  ( 24.95276293194433492, -10.68636129284900704, 14.88498244535527881 ) ) ;
#3551 = VECTOR ( 'NONE', #19288, 1000.000000000000000 ) ;
#3552 = ADVANCED_FACE ( 'NONE', ( #6958 ), #16476, .F. ) ;
#3553 = CARTESIAN_POINT ( 'NONE',  ( 0.000000000000000000, 0.000000000000000000, 293.5832628385307999 ) ) ;
#3554 = AXIS2_PLACEMENT_3D ( 'NONE', #9157, #20102, #12316 ) ;
#3555 = LINE ( 'NONE', #9786, #16474 ) ;
#3556 = LINE ( 'NONE', #8047, #13965 ) ;
#3557 = ORIENTED_EDGE ( 'NONE', *, *, #2423, .F. ) ;
#3558 = FACE_OUTER_BOUND ( 'NONE', #9060, .T. ) ;
#3559 = DIRECTION ( 'NONE',  ( 0.3747554100459959958, 0.9271237148521535021, 0.000000000000000000 ) ) ;
#3560 = ORIENTED_EDGE ( 'NONE', *, *, #9396, .F. ) ;
#3561 = FACE_OUTER_BOUND ( 'NONE', #18777, .T. ) ;
#3562 = DIRECTION ( 'NONE',  ( 0.000000000000000000, 0.000000000000000000, -1.000000000000000000 ) ) ;
#3563 = FACE_BOUND ( 'NONE', #12463, .T. ) ;
#3564 = DIRECTION ( 'NONE',  ( 1.000000000000000000, 0.000000000000000000, -6.994638739193269649E-15 ) ) ;
#3565 = CARTESIAN_POINT ( 'NONE',  ( -141.6227766016837961, -18.73072656238141320, -9.999999999999985789 ) ) ;
#3566 = FACE_OUTER_BOUND ( 'NONE', #14809, .T. ) ;
#3567 = DIRECTION ( 'NONE',  ( -1.000000000000000000, 0.000000000000000000, 0.000000000000000000 ) ) ;
#3568 = VECTOR ( 'NONE', #3852, 1000.000000000000227 ) ;
#3569 = CIRCLE ( 'NONE', #3896, 150.0000000000000284 ) ;
#3570 = ORIENTED_EDGE ( 'NONE', *, *, #121, .F. ) ;
#3571 = AXIS2_PLACEMENT_3D ( 'NONE', #13147, #16445, #876 ) ;
#3572 = CARTESIAN_POINT ( 'NONE',  ( 8.939227532413712041, -60.08331549348429235, 293.5832628385307999 ) ) ;
#3573 = ORIENTED_EDGE ( 'NONE', *, *, #19996, .F. ) ;
#3574 = ORIENTED_EDGE ( 'NONE', *, *, #4802, .T. ) ;
#3575 = CARTESIAN_POINT ( 'NONE',  ( 7.350000000000000533, 9.000000000000000000, 0.000000000000000000 ) ) ;
#3576 = ORIENTED_EDGE ( 'NONE', *, *, #5014, .F. ) ;
#3577 = PLANE ( 'NONE',  #922 ) ;
#3578 = FACE_BOUND ( 'NONE', #16226, .T. ) ;
#3579 = ORIENTED_EDGE ( 'NONE', *, *, #20008, .T. ) ;
#3580 = FACE_OUTER_BOUND ( 'NONE', #13716, .T. ) ;
#3581 = DIRECTION ( 'NONE',  ( -0.9781142164131917394, 0.2080686897406911207, 0.000000000000000000 ) ) ;
#3582 = VECTOR ( 'NONE', #6478, 1000.000000000000227 ) ;
#3583 = CIRCLE ( 'NONE', #8162, 7.500000000000008882 ) ;
#3584 = LINE ( 'NONE', #8075, #3957 ) ;
#3585 = CARTESIAN_POINT ( 'NONE',  ( 106.5749805965075012, -120.1845445602442339, 7.623296525288700586E-17 ) ) ;
#3586 = LINE ( 'NONE', #14626, #8524 ) ;
#3587 = CYLINDRICAL_SURFACE ( 'NONE', #15495, 9.000000000000001776 ) ;
#3588 = VERTEX_POINT ( 'NONE', #6861 ) ;
#3589 = CARTESIAN_POINT ( 'NONE',  ( 4.189777606611760026E-13, -60.00000000000000000, -105.0000000000000142 ) ) ;
#3590 = APPLICATION_CONTEXT ( 'automotive_design' ) ;
#3591 = CARTESIAN_POINT ( 'NONE',  ( 0.000000000000000000, 0.000000000000000000, 293.5832628385307999 ) ) ;
#3592 = CYLINDRICAL_SURFACE ( 'NONE', #9800, 127.4413876050234649 ) ;
#3593 = CARTESIAN_POINT ( 'NONE',  ( 99.34007343273268020, -112.3954413154693839, 39.16393061809239384 ) ) ;
#3594 = ORIENTED_EDGE ( 'NONE', *, *, #745, .F. ) ;
#3595 = DIRECTION ( 'NONE',  ( -4.650550193362991910E-16, -1.000000000000000000, 0.000000000000000000 ) ) ;
#3596 = CARTESIAN_POINT ( 'NONE',  ( -108.7690249705941596, 103.3081676305584864, 44.99999999999997868 ) ) ;
#3597 = ORIENTED_EDGE ( 'NONE', *, *, #4601, .F. ) ;
#3598 = CIRCLE ( 'NONE', #2256, 112.8770930172170637 ) ;
#3599 = EDGE_LOOP ( 'NONE', ( #169, #404, #13090, #7161 ) ) ;
#3600 = ORIENTED_EDGE ( 'NONE', *, *, #5903, .F. ) ;
#3601 = ORIENTED_EDGE ( 'NONE', *, *, #6285, .T. ) ;
#3602 = EDGE_CURVE ( 'NONE', #2811, #14900, #16572, .T. ) ;
#3603 = CARTESIAN_POINT ( 'NONE',  ( -149.6019236298159569, 11.14724313840852155, 10.74694859380678302 ) ) ;
#3604 = VERTEX_POINT ( 'NONE', #5234 ) ;
#3605 = CARTESIAN_POINT ( 'NONE',  ( 45.84586732611860782, -36.66871011346395193, 132.4711112102474146 ) ) ;
#3606 = CARTESIAN_POINT ( 'NONE',  ( -85.53020504959707182, -140.9188050298390067, 49.99999999999999289 ) ) ;
#3607 = CARTESIAN_POINT ( 'NONE',  ( -95.54911406155835607, -115.6381493485951069, -9.242025372095096003 ) ) ;
#3608 = ORIENTED_EDGE ( 'NONE', *, *, #11479, .T. ) ;
#3609 = CIRCLE ( 'NONE', #15362, 7.500000000000001776 ) ;
#3610 =( GEOMETRIC_REPRESENTATION_CONTEXT ( 3 ) GLOBAL_UNCERTAINTY_ASSIGNED_CONTEXT ( ( #6235 ) ) GLOBAL_UNIT_ASSIGNED_CONTEXT ( ( #13510, #5655, #13305 ) ) REPRESENTATION_CONTEXT ( 'NONE', 'WORKASPACE' ) );
#3611 = AXIS2_PLACEMENT_3D ( 'NONE', #13397, #8309, #2285 ) ;
#3612 = DIRECTION ( 'NONE',  ( -6.982962677686266711E-15, 0.000000000000000000, -1.000000000000000000 ) ) ;
#3613 = FACE_BOUND ( 'NONE', #6450, .T. ) ;
#3614 = EDGE_CURVE ( 'NONE', #14025, #17652, #14159, .T. ) ;
#3615 = DIRECTION ( 'NONE',  ( -0.000000000000000000, -0.000000000000000000, 1.000000000000000000 ) ) ;
#3616 = EDGE_CURVE ( 'NONE', #8266, #8936, #9928, .T. ) ;
#3617 = FACE_OUTER_BOUND ( 'NONE', #19792, .T. ) ;
#3618 = CARTESIAN_POINT ( 'NONE',  ( -5.524863963826822655, -116.0870680293436408, 14.88498244535549020 ) ) ;
#3619 = CARTESIAN_POINT ( 'NONE',  ( 0.000000000000000000, 0.000000000000000000, -100.0000000000000000 ) ) ;
#3620 = VERTEX_POINT ( 'NONE', #14922 ) ;
#3621 = EDGE_CURVE ( 'NONE', #13255, #2196, #16176, .T. ) ;
#3622 = PRODUCT ( 'Vane Disc', 'Vane Disc', '', ( #17526 ) ) ;
#3623 = CARTESIAN_POINT ( 'NONE',  ( -132.9093122671970093, 36.24889438955336374, -21.52074723781268872 ) ) ;
#3624 = ORIENTED_EDGE ( 'NONE', *, *, #3298, .T. ) ;
#3625 = AXIS2_PLACEMENT_3D ( 'NONE', #3972, #5131, #11355 ) ;
#3626 = ORIENTED_EDGE ( 'NONE', *, *, #8233, .F. ) ;
#3627 = ADVANCED_FACE ( 'NONE', ( #7164 ), #14631, .T. ) ;
#3628 = ORIENTED_EDGE ( 'NONE', *, *, #8222, .T. ) ;
#3629 = CARTESIAN_POINT ( 'NONE',  ( -79.75827554147308263, 0.000000000000000000, 269.6944534026102360 ) ) ;
#3630 = CARTESIAN_POINT ( 'NONE',  ( 53.86996498385652643, 28.06584155524120305, 283.5832628385307999 ) ) ;
#3631 = CARTESIAN_POINT ( 'NONE',  ( -67.36461649554505016, 39.84224160888970800, 132.4711112102474146 ) ) ;
#3632 = CARTESIAN_POINT ( 'NONE',  ( -135.7697856077824667, -31.23579568862577815, -16.57641459956559515 ) ) ;
#3633 = CYLINDRICAL_SURFACE ( 'NONE', #614, 7.500000000000006217 ) ;
#3634 = AXIS2_PLACEMENT_3D ( 'NONE', #9694, #17487, #19023 ) ;
#3635 = CARTESIAN_POINT ( 'NONE',  ( -53.86996498385652643, -28.06584155524119595, 293.5832628385307999 ) ) ;
#3636 = DIRECTION ( 'NONE',  ( 1.000000000000000000, 0.000000000000000000, -0.000000000000000000 ) ) ;
#3637 = EDGE_CURVE ( 'NONE', #7218, #11048, #19342, .T. ) ;
#3638 = DIRECTION ( 'NONE',  ( 6.982962677686266711E-15, -0.000000000000000000, 1.000000000000000000 ) ) ;
#3639 = AXIS2_PLACEMENT_3D ( 'NONE', #5062, #11284, #4960 ) ;
#3640 = DIRECTION ( 'NONE',  ( -0.000000000000000000, -0.000000000000000000, 1.000000000000000000 ) ) ;
#3641 = EDGE_CURVE ( 'NONE', #6330, #6851, #3609, .T. ) ;
#3642 = EDGE_LOOP ( 'NONE', ( #9938, #13927 ) ) ;
#3643 = CARTESIAN_POINT ( 'NONE',  ( 130.9868171408399746, -91.88282611735537841, 40.00000000000000000 ) ) ;
#3644 = ORIENTED_EDGE ( 'NONE', *, *, #19854, .T. ) ;
#3645 = ORIENTED_EDGE ( 'NONE', *, *, #8360, .F. ) ;
#3646 = EDGE_LOOP ( 'NONE', ( #4892, #9590, #6375, #13046 ) ) ;
#3647 = ORIENTED_EDGE ( 'NONE', *, *, #20232, .T. ) ;
#3648 = CARTESIAN_POINT ( 'NONE',  ( 53.86996498385654064, 28.06584155524121016, 293.5832628385307999 ) ) ;
#3649 = EDGE_CURVE ( 'NONE', #2972, #5912, #1208, .T. ) ;
#3650 = ORIENTED_EDGE ( 'NONE', *, *, #9118, .F. ) ;
#3651 = CARTESIAN_POINT ( 'NONE',  ( -37.93579148621510200, -68.46530598706787885, 132.4711112102474146 ) ) ;
#3652 = CARTESIAN_POINT ( 'NONE',  ( -59.42266395395758849, 50.93469132750324491, 132.4711112102474146 ) ) ;
#3653 = DIRECTION ( 'NONE',  ( -0.4693298356057531429, 0.8830229359480288309, 0.000000000000000000 ) ) ;
#3654 = FACE_OUTER_BOUND ( 'NONE', #2393, .T. ) ;
#3655 = ORIENTED_EDGE ( 'NONE', *, *, #17655, .F. ) ;
#3656 = CARTESIAN_POINT ( 'NONE',  ( 106.5208805777954524, 53.25886146954521649, 39.88498244535470860 ) ) ;
#3657 = CARTESIAN_POINT ( 'NONE',  ( 0.000000000000000000, 0.000000000000000000, 0.000000000000000000 ) ) ;
#3658 = EDGE_LOOP ( 'NONE', ( #18419, #14498, #16680, #15748 ) ) ;
#3659 = DIRECTION ( 'NONE',  ( 1.613511099790691498E-16, -1.000000000000000000, 0.000000000000000000 ) ) ;
#3660 = FACE_OUTER_BOUND ( 'NONE', #8884, .T. ) ;
#3661 = ADVANCED_FACE ( 'NONE', ( #20134 ), #13476, .F. ) ;
#3662 = CARTESIAN_POINT ( 'NONE',  ( 0.000000000000000000, 0.000000000000000000, 248.9926560891072143 ) ) ;
#3663 = EDGE_CURVE ( 'NONE', #10563, #108, #8879, .T. ) ;
#3664 = CARTESIAN_POINT ( 'NONE',  ( -134.5971911056698502, -73.88063391572673311, 32.93306624859282294 ) ) ;
#3665 = CARTESIAN_POINT ( 'NONE',  ( -136.6495813276215472, -27.08701270267532024, -17.69344187970681403 ) ) ;
#3666 = PLANE ( 'NONE',  #8894 ) ;
#3667 = CARTESIAN_POINT ( 'NONE',  ( -76.10696272933056150, 117.5065231191640009, -3.774081802667871521 ) ) ;
#3668 = EDGE_CURVE ( 'NONE', #8563, #16678, #18198, .T. ) ;
#3669 = EDGE_LOOP ( 'NONE', ( #17242, #8196, #11928, #19491 ) ) ;
#3670 = LINE ( 'NONE', #11631, #12177 ) ;
#3671 = AXIS2_PLACEMENT_3D ( 'NONE', #15794, #3615, #6490 ) ;
#3672 = ORIENTED_EDGE ( 'NONE', *, *, #18599, .F. ) ;
#3673 = VERTEX_POINT ( 'NONE', #4179 ) ;
#3674 = DIRECTION ( 'NONE',  ( 1.000000000000000000, 0.000000000000000000, 0.000000000000000000 ) ) ;
#3675 = ORIENTED_EDGE ( 'NONE', *, *, #15885, .T. ) ;
#3676 = CARTESIAN_POINT ( 'NONE',  ( 9.401191644521611934, 61.25984398917705676, 248.9926560891072143 ) ) ;
#3677 = CARTESIAN_POINT ( 'NONE',  ( -89.19226148815702970, -120.6070458769191589, 45.77850350706554394 ) ) ;
#3678 = CARTESIAN_POINT ( 'NONE',  ( 0.000000000000000000, 0.000000000000000000, 293.5832628385307999 ) ) ;
#3679 = DIRECTION ( 'NONE',  ( -0.000000000000000000, -0.000000000000000000, -1.000000000000000000 ) ) ;
#3680 = LINE ( 'NONE', #19335, #7385 ) ;
#3682 = AXIS2_PLACEMENT_3D ( 'NONE', #14608, #13060, #5304 ) ;
#3681 = CARTESIAN_POINT ( 'NONE',  ( 25.47058595421554372, 74.01264520835162841, 132.4711112102474146 ) ) ;
#3683 = AXIS2_PLACEMENT_3D ( 'NONE', #3686, #17908, #2352 ) ;
#3684 = CYLINDRICAL_SURFACE ( 'NONE', #17994, 112.8770930172170210 ) ;
#3685 = DIRECTION ( 'NONE',  ( -0.000000000000000000, -0.000000000000000000, 1.000000000000000000 ) ) ;
#3686 = CARTESIAN_POINT ( 'NONE',  ( 0.000000000000000000, 0.000000000000000000, 132.4711112102474146 ) ) ;
#3687 = DIRECTION ( 'NONE',  ( 0.000000000000000000, 0.000000000000000000, 1.000000000000000000 ) ) ;
#3688 = CARTESIAN_POINT ( 'NONE',  ( 86.50547518363042343, -122.5441694604242429, -2.983597003230881839 ) ) ;
#3689 = CARTESIAN_POINT ( 'NONE',  ( 100.0291087223604762, -111.7819692016171302, 39.61901476276965894 ) ) ;
#3690 = EDGE_CURVE ( 'NONE', #5360, #5032, #15123, .T. ) ;
#3691 = ORIENTED_EDGE ( 'NONE', *, *, #12193, .F. ) ;
#3692 = CARTESIAN_POINT ( 'NONE',  ( 71.18887634719571622, -147.8252249328912740, 39.99999999999999289 ) ) ;
#3693 = CARTESIAN_POINT ( 'NONE',  ( -107.5112643209296976, 104.6166421110821432, 44.94337129641210993 ) ) ;
#3694 = VERTEX_POINT ( 'NONE', #10819 ) ;
#3695 = VERTEX_POINT ( 'NONE', #16669 ) ;
#3696 = ORIENTED_EDGE ( 'NONE', *, *, #6418, .F. ) ;
#3697 = APPLICATION_PROTOCOL_DEFINITION ( 'draft international standard', 'automotive_design', 1998, #13758 ) ;
#3698 = AXIS2_PLACEMENT_3D ( 'NONE', #7089, #4006, #5453 ) ;
#3699 = CIRCLE ( 'NONE', #14151, 7.500000000000020428 ) ;
#3700 = VERTEX_POINT ( 'NONE', #15326 ) ;
#3701 = CARTESIAN_POINT ( 'NONE',  ( -143.3909699111413545, 44.26766431025286153, 27.15461939389479085 ) ) ;
#3702 = ORIENTED_EDGE ( 'NONE', *, *, #4419, .T. ) ;
#3703 = AXIS2_PLACEMENT_3D ( 'NONE', #3446, #3343, #10801 ) ;
#3704 = CARTESIAN_POINT ( 'NONE',  ( 5.590028426173794251, 1.289614712049196976, 293.5832628385307999 ) ) ;
#3705 = CARTESIAN_POINT ( 'NONE',  ( 0.3570196857253503664, 9.540868182094907723, 1.474731560294323396 ) ) ;
#3706 = CARTESIAN_POINT ( 'NONE',  ( -84.44144489237834250, -123.9750712224044236, 0.1650835480906647224 ) ) ;
#3707 = ORIENTED_EDGE ( 'NONE', *, *, #6423, .T. ) ;
#3708 = CARTESIAN_POINT ( 'NONE',  ( -138.4462077254157748, -20.96029677485602960, 25.40435766516374017 ) ) ;
#3709 = CARTESIAN_POINT ( 'NONE',  ( 7.350000000000001421, -7.794228634059936489, 4.500000000000017764 ) ) ;
#3710 = CIRCLE ( 'NONE', #16124, 7.500000000000007105 ) ;
#3711 =( LENGTH_UNIT ( ) NAMED_UNIT ( * ) SI_UNIT ( .MILLI., .METRE. ) );
#3712 = LINE ( 'NONE', #737, #15318 ) ;
#3713 = CYLINDRICAL_SURFACE ( 'NONE', #13550, 62.91752772691707207 ) ;
#3714 = ADVANCED_FACE ( 'NONE', ( #17075 ), #7446, .T. ) ;
#3715 = ORIENTED_EDGE ( 'NONE', *, *, #3155, .T. ) ;
#3716 = DIRECTION ( 'NONE',  ( 1.000000000000000000, 0.000000000000000000, 0.000000000000000000 ) ) ;
#3717 = VECTOR ( 'NONE', #14763, 1000.000000000000000 ) ;
#3718 = B_SPLINE_CURVE_WITH_KNOTS ( 'NONE', 3,
 ( #12826, #12728, #14064, #4970, #14373, #349 ),
 .UNSPECIFIED., .F., .F.,
 ( 4, 2, 4 ),
 ( 2.380730970505090493E-07, 0.002629065763328468884, 0.005257893453559887159 ),
 .UNSPECIFIED. ) ;
#3719 = PRESENTATION_LAYER_ASSIGNMENT (  '', '', ( #5053 ) ) ;
#3720 = VERTEX_POINT ( 'NONE', #13578 ) ;
#3721 = VERTEX_POINT ( 'NONE', #12043 ) ;
#3722 = ADVANCED_FACE ( 'NONE', ( #18304 ), #4282, .F. ) ;
#3723 = DIRECTION ( 'NONE',  ( 0.000000000000000000, 0.000000000000000000, 1.000000000000000000 ) ) ;
#3724 = CARTESIAN_POINT ( 'NONE',  ( -109.9999999999983515, 275.0000000000000000, 77.50000000000000000 ) ) ;
#3725 = VECTOR ( 'NONE', #12397, 1000.000000000000000 ) ;
#3726 = DIRECTION ( 'NONE',  ( 1.000000000000000000, 0.000000000000000000, 0.000000000000000000 ) ) ;
#3727 = PLANE ( 'NONE',  #6176 ) ;
#3728 = CYLINDRICAL_SURFACE ( 'NONE', #3772, 7.500000000000007105 ) ;
#3729 = DIRECTION ( 'NONE',  ( 6.982962677686266711E-15, -0.000000000000000000, 1.000000000000000000 ) ) ;
#3730 = CARTESIAN_POINT ( 'NONE',  ( 77.21438937758500742, 12.78021302872875431, 132.4711112102474146 ) ) ;
#3731 = CARTESIAN_POINT ( 'NONE',  ( 102.6608643076873335, -126.6195776799898312, 38.76864583652064766 ) ) ;
#3732 = DIRECTION ( 'NONE',  ( 0.7818314824680226982, 0.6234898018587423651, 0.000000000000000000 ) ) ;
#3733 = EDGE_CURVE ( 'NONE', #7708, #7514, #7842, .T. ) ;
#3734 = VERTEX_POINT ( 'NONE', #10610 ) ;
#3735 = ORIENTED_EDGE ( 'NONE', *, *, #3742, .T. ) ;
#3736 = ORIENTED_EDGE ( 'NONE', *, *, #3533, .F. ) ;
#3737 = EDGE_LOOP ( 'NONE', ( #13111, #1035, #4240, #17971 ) ) ;
#3738 = COLOUR_RGB ( '', 0.66274510, 0.83137255, 0.94901961) ;
#3739 = ORIENTED_EDGE ( 'NONE', *, *, #5014, .T. ) ;
#3740 = ADVANCED_FACE ( 'NONE', ( #9083 ), #11128, .F. ) ;
#3741 = VERTEX_POINT ( 'NONE', #11230 ) ;
#3742 = EDGE_CURVE ( 'NONE', #4464, #14482, #17389, .T. ) ;
#3743 = FACE_OUTER_BOUND ( 'NONE', #2277, .T. ) ;
#3744 = LINE ( 'NONE', #8451, #5686 ) ;
#3745 = CARTESIAN_POINT ( 'NONE',  ( 156.4179374840099683, -52.02840013023883614, 39.99999999999999289 ) ) ;
#3746 = ORIENTED_EDGE ( 'NONE', *, *, #12878, .F. ) ;
#3748 = DIRECTION ( 'NONE',  ( -0.6155349844899689060, 0.7881095627315620744, 0.000000000000000000 ) ) ;
#3747 = AXIS2_PLACEMENT_3D ( 'NONE', #15837, #15785, #6483 ) ;
#3749 = CARTESIAN_POINT ( 'NONE',  ( 79.05640494598117129, -127.4758205975433327, 49.99999999999999289 ) ) ;
#3750 = ORIENTED_EDGE ( 'NONE', *, *, #17136, .T. ) ;
#3751 = CARTESIAN_POINT ( 'NONE',  ( 0.8038475772933695307, 10.39230484541327471, -5.094467845664485666E-17 ) ) ;
#3752 = CARTESIAN_POINT ( 'NONE',  ( 30.74413178637190924, -54.89456854707551514, 248.9926560891072143 ) ) ;
#3753 = AXIS2_PLACEMENT_3D ( 'NONE', #18055, #4031, #12092 ) ;
#3754 = LINE ( 'NONE', #16248, #5914 ) ;
#3755 = EDGE_CURVE ( 'NONE', #14163, #14818, #13995, .T. ) ;
#3756 = CARTESIAN_POINT ( 'NONE',  ( -167.4599531637108782, -36.50981547337168109, 60.00000000000000000 ) ) ;
#3757 = CARTESIAN_POINT ( 'NONE',  ( 105.9946577255053626, 51.49356311920430329, 14.88498244535471215 ) ) ;
#3758 = FACE_OUTER_BOUND ( 'NONE', #9626, .T. ) ;
#3759 = ORIENTED_EDGE ( 'NONE', *, *, #16980, .T. ) ;
#3760 = DIRECTION ( 'NONE',  ( -0.000000000000000000, -0.000000000000000000, -1.000000000000000000 ) ) ;
#3761 = ORIENTED_EDGE ( 'NONE', *, *, #3131, .T. ) ;
#3762 = AXIS2_PLACEMENT_3D ( 'NONE', #4714, #9414, #1646 ) ;
#3763 = ORIENTED_EDGE ( 'NONE', *, *, #11892, .T. ) ;
#3764 = CARTESIAN_POINT ( 'NONE',  ( -50.37374754117255549, -141.2886604036510221, 60.00000000000000000 ) ) ;
#3765 = ORIENTED_EDGE ( 'NONE', *, *, #294, .T. ) ;
#3766 = ADVANCED_FACE ( 'NONE', ( #7959 ), #6642, .F. ) ;
#3767 = ADVANCED_FACE ( 'NONE', ( #12867 ), #9698, .T. ) ;
#3768 = CARTESIAN_POINT ( 'NONE',  ( -110.0000000000000142, 275.0000000000000568, 5.000000000000000888 ) ) ;
#3769 = PLANE ( 'NONE',  #14825 ) ;
#3770 = LINE ( 'NONE', #5415, #5109 ) ;
#3771 = FACE_OUTER_BOUND ( 'NONE', #14291, .T. ) ;
#3772 = AXIS2_PLACEMENT_3D ( 'NONE', #11787, #8830, #10070 ) ;
#3773 = VERTEX_POINT ( 'NONE', #10925 ) ;
#3774 = DIRECTION ( 'NONE',  ( 0.2080686897406943681, 0.9781142164131909622, 0.000000000000000000 ) ) ;
#3775 = CARTESIAN_POINT ( 'NONE',  ( 134.1130761623740568, -69.50842595698583182, 49.99999999999999289 ) ) ;
#3776 = AXIS2_PLACEMENT_3D ( 'NONE', #6481, #19070, #11273 ) ;
#3777 = PLANE ( 'NONE',  #19615 ) ;
#3778 = DIRECTION ( 'NONE',  ( 0.4693298356057531984, -0.8830229359480288309, 0.000000000000000000 ) ) ;
#3779 = ORIENTED_EDGE ( 'NONE', *, *, #5127, .T. ) ;
#3780 = DIRECTION ( 'NONE',  ( 1.000000000000000000, 0.000000000000000000, 0.000000000000000000 ) ) ;
#3781 = EDGE_CURVE ( 'NONE', #7108, #17239, #3364, .T. ) ;
#3782 = CYLINDRICAL_SURFACE ( 'NONE', #11661, 3.224098631618460331 ) ;
#3783 = DIRECTION ( 'NONE',  ( 0.8660254037844380415, 0.5000000000000009992, 0.000000000000000000 ) ) ;
#3784 = FACE_BOUND ( 'NONE', #10674, .T. ) ;
#3785 = ORIENTED_EDGE ( 'NONE', *, *, #15653, .T. ) ;
#3786 = CARTESIAN_POINT ( 'NONE',  ( 0.000000000000000000, 0.000000000000000000, 132.4711112102474146 ) ) ;
#3787 = DIRECTION ( 'NONE',  ( 0.000000000000000000, 1.000000000000000000, 0.000000000000000000 ) ) ;
#3788 = ORIENTED_EDGE ( 'NONE', *, *, #19393, .F. ) ;
#3789 = AXIS2_PLACEMENT_3D ( 'NONE', #20182, #6075, #2693 ) ;
#3790 = VERTEX_POINT ( 'NONE', #1934 ) ;
#3791 = EDGE_LOOP ( 'NONE', ( #17768, #10295, #4662, #652 ) ) ;
#3792 = ITEM_DEFINED_TRANSFORMATION ( 'NONE', 'NONE', #19012,  #18639 ) ;
#3793 = EDGE_CURVE ( 'NONE', #1302, #3741, #4578, .T. ) ;
#3794 = ORIENTED_EDGE ( 'NONE', *, *, #2779, .T. ) ;
#3795 = AXIS2_PLACEMENT_3D ( 'NONE', #14091, #5814, #9688 ) ;
#3796 = DIRECTION ( 'NONE',  ( 1.000000000000000000, 0.000000000000000000, 0.000000000000000000 ) ) ;
#3797 = ORIENTED_EDGE ( 'NONE', *, *, #4544, .F. ) ;
#3798 = SURFACE_SIDE_STYLE ('',( #12906 ) ) ;
#3799 = DIRECTION ( 'NONE',  ( 0.000000000000000000, 1.000000000000000000, 0.000000000000000000 ) ) ;
#3800 = CARTESIAN_POINT ( 'NONE',  ( -84.96040761327874691, -123.6194689893696932, -0.7396600334858707271 ) ) ;
#3801 = EDGE_LOOP ( 'NONE', ( #2712, #9678, #676, #12389 ) ) ;
#3802 = ADVANCED_FACE ( 'NONE', ( #14409 ), #390, .T. ) ;
#3803 = VECTOR ( 'NONE', #4587, 1000.000000000000227 ) ;
#3804 = DIRECTION ( 'NONE',  ( 0.000000000000000000, -1.000000000000000000, -1.734723475976808080E-16 ) ) ;
#3805 = DIRECTION ( 'NONE',  ( -0.000000000000000000, 1.000000000000000000, -0.000000000000000000 ) ) ;
#3806 = VECTOR ( 'NONE', #20069, 1000.000000000000000 ) ;
#3807 = DIRECTION ( 'NONE',  ( -1.000000000000000000, 0.000000000000000000, 0.000000000000000000 ) ) ;
#3808 = DIRECTION ( 'NONE',  ( -0.9848077530122085754, 0.1736481776669273336, 0.000000000000000000 ) ) ;
#3809 = DIRECTION ( 'NONE',  ( 0.000000000000000000, 0.000000000000000000, -1.000000000000000000 ) ) ;
#3810 = PLANE ( 'NONE',  #13883 ) ;
#3811 = ORIENTED_EDGE ( 'NONE', *, *, #14489, .T. ) ;
#3812 = AXIS2_PLACEMENT_3D ( 'NONE', #14386, #6616, #8035 ) ;
#3813 = DIRECTION ( 'NONE',  ( -0.1390141521205912334, 0.9902903945359629034, 0.000000000000000000 ) ) ;
#3814 = CARTESIAN_POINT ( 'NONE',  ( -56.50138340076688337, 22.29928840491054487, 293.5832628385307999 ) ) ;
#3815 = AXIS2_PLACEMENT_3D ( 'NONE', #14069, #17047, #19901 ) ;
#3816 = ORIENTED_EDGE ( 'NONE', *, *, #18532, .T. ) ;
#3817 = B_SPLINE_CURVE_WITH_KNOTS ( 'NONE', 3,
 ( #17063, #10702, #9386, #6020, #16958, #9176, #12237, #3151 ),
 .UNSPECIFIED., .F., .F.,
 ( 4, 2, 2, 4 ),
 ( 0.005257893453559910578, 0.006567392922673243386, 0.007876892391786575326, 0.01049589133001324268 ),
 .UNSPECIFIED. ) ;
#3818 = VERTEX_POINT ( 'NONE', #6240 ) ;
#3819 = DIRECTION ( 'NONE',  ( 0.7071067811865472397, 0.000000000000000000, 0.7071067811865479058 ) ) ;
#3820 = AXIS2_PLACEMENT_3D ( 'NONE', #5233, #8386, #11458 ) ;
#3821 = CARTESIAN_POINT ( 'NONE',  ( -128.8937720816053627, -76.72575536401159013, -7.584633839317217685 ) ) ;
#3822 = AXIS2_PLACEMENT_3D ( 'NONE', #13226, #17961, #5570 ) ;
#3823 = CARTESIAN_POINT ( 'NONE',  ( -78.26059000578311498, -1.379293853802032732, 248.9926560891072143 ) ) ;
#3824 = DIRECTION ( 'NONE',  ( 1.000000000000000000, 0.000000000000000000, -0.000000000000000000 ) ) ;
#3825 = ORIENTED_EDGE ( 'NONE', *, *, #3853, .F. ) ;
#3826 = DIRECTION ( 'NONE',  ( 0.000000000000000000, 0.000000000000000000, 1.000000000000000000 ) ) ;
#3827 = CARTESIAN_POINT ( 'NONE',  ( -131.7825524766324179, -71.64958008132045109, -3.998968123500318939 ) ) ;
#3828 = CARTESIAN_POINT ( 'NONE',  ( 135.1060089022256818, -65.16414933467422088, 10.00000000000000888 ) ) ;
#3829 = DIRECTION ( 'NONE',  ( -0.000000000000000000, -0.000000000000000000, -1.000000000000000000 ) ) ;
#3830 = DIRECTION ( 'NONE',  ( -0.9902903945359630145, -0.1390141521205912334, 0.000000000000000000 ) ) ;
#3831 = VERTEX_POINT ( 'NONE', #11338 ) ;
#3832 = AXIS2_PLACEMENT_3D ( 'NONE', #7639, #6229, #2846 ) ;
#3834 = ORIENTED_EDGE ( 'NONE', *, *, #6019, .F. ) ;
#3833 = CIRCLE ( 'NONE', #6468, 150.0000000000000284 ) ;
#3835 = CIRCLE ( 'NONE', #7113, 112.8770930172170068 ) ;
#3836 = EDGE_LOOP ( 'NONE', ( #20021, #13092, #3889, #2591 ) ) ;
#3837 = ORIENTED_EDGE ( 'NONE', *, *, #10862, .T. ) ;
#3838 = FACE_OUTER_BOUND ( 'NONE', #8072, .T. ) ;
#3839 = ORIENTED_EDGE ( 'NONE', *, *, #12097, .F. ) ;
#3840 = EDGE_CURVE ( 'NONE', #3915, #6246, #17184, .T. ) ;
#3841 = CARTESIAN_POINT ( 'NONE',  ( -20.69304990905115815, 6.063840362151032615, 248.9926560891072143 ) ) ;
#3842 = LINE ( 'NONE', #19498, #19724 ) ;
#3843 = FACE_OUTER_BOUND ( 'NONE', #10309, .T. ) ;
#3844 = ORIENTED_EDGE ( 'NONE', *, *, #16132, .F. ) ;
#3845 = CARTESIAN_POINT ( 'NONE',  ( -52.50000000000000000, -2.094888803305880013E-13, -100.0000000000000000 ) ) ;
#3846 = LINE ( 'NONE', #2127, #8144 ) ;
#3847 = AXIS2_PLACEMENT_3D ( 'NONE', #4446, #10677, #9151 ) ;
#3848 = ORIENTED_EDGE ( 'NONE', *, *, #10883, .F. ) ;
#3849 = CARTESIAN_POINT ( 'NONE',  ( 0.000000000000000000, 0.000000000000000000, 0.000000000000000000 ) ) ;
#3850 = AXIS2_PLACEMENT_3D ( 'NONE', #12740, #19000, #17466 ) ;
#3851 = FACE_OUTER_BOUND ( 'NONE', #10208, .T. ) ;
#3852 = DIRECTION ( 'NONE',  ( -0.9749279121818223981, -0.2225209339563194721, 0.000000000000000000 ) ) ;
#3853 = EDGE_CURVE ( 'NONE', #3346, #18071, #975, .T. ) ;
#3854 = DIRECTION ( 'NONE',  ( 0.000000000000000000, 0.000000000000000000, 1.000000000000000000 ) ) ;
#3855 = EDGE_CURVE ( 'NONE', #4788, #2109, #15644, .T. ) ;
#3856 = EDGE_CURVE ( 'NONE', #11985, #15095, #12559, .T. ) ;
#3857 = CARTESIAN_POINT ( 'NONE',  ( 0.000000000000000000, 60.00000000000000000, -105.0000000000000142 ) ) ;
#3858 = CARTESIAN_POINT ( 'NONE',  ( 135.7779226595531270, 102.2982297021113141, 49.99999999999999289 ) ) ;
#3859 = LINE ( 'NONE', #8464, #5451 ) ;
#3860 = ORIENTED_EDGE ( 'NONE', *, *, #11561, .T. ) ;
#3861 = EDGE_CURVE ( 'NONE', #19610, #6772, #11026, .T. ) ;
#3862 = DIRECTION ( 'NONE',  ( 1.000000000000000000, 0.000000000000000000, 0.000000000000000000 ) ) ;
#3863 = CIRCLE ( 'NONE', #8760, 17.50000000000000355 ) ;
#3864 = ORIENTED_EDGE ( 'NONE', *, *, #5035, .T. ) ;
#3865 = AXIS2_PLACEMENT_3D ( 'NONE', #18551, #4426, #1043 ) ;
#3866 = ORIENTED_EDGE ( 'NONE', *, *, #15885, .F. ) ;
#3867 = CARTESIAN_POINT ( 'NONE',  ( -4.811834253409058348, -3.123743752084112035, 293.5832628385307999 ) ) ;
#3868 = CIRCLE ( 'NONE', #15296, 60.74260934110282051 ) ;
#3869 = ORIENTED_EDGE ( 'NONE', *, *, #5675, .F. ) ;
#3870 = EDGE_CURVE ( 'NONE', #7406, #3444, #2624, .T. ) ;
#3871 = DIRECTION ( 'NONE',  ( 0.1736481776669172583, 0.9848077530122103518, 0.000000000000000000 ) ) ;
#3872 = DIRECTION ( 'NONE',  ( 1.000000000000000000, 0.000000000000000000, -0.000000000000000000 ) ) ;
#3873 = LINE ( 'NONE', #8575, #13558 ) ;
#3874 = DIRECTION ( 'NONE',  ( -0.000000000000000000, -0.000000000000000000, -1.000000000000000000 ) ) ;
#3875 = VERTEX_POINT ( 'NONE', #2333 ) ;
#3876 = DIRECTION ( 'NONE',  ( 0.000000000000000000, 0.000000000000000000, 1.000000000000000000 ) ) ;
#3877 = CARTESIAN_POINT ( 'NONE',  ( 97.53506906366369833, -133.9085396777615244, 9.038951145123888864 ) ) ;
#3878 = AXIS2_PLACEMENT_3D ( 'NONE', #3253, #2947, #4577 ) ;
#3879 = VECTOR ( 'NONE', #9498, 1000.000000000000000 ) ;
#3880 = CARTESIAN_POINT ( 'NONE',  ( -79.05640494597940915, -127.4758205975444270, 60.00000000000000000 ) ) ;
#3881 = CARTESIAN_POINT ( 'NONE',  ( -71.18887634719365565, -147.8252249328922687, 39.99999999999999289 ) ) ;
#3882 = VECTOR ( 'NONE', #9667, 1000.000000000000000 ) ;
#3883 = ORIENTED_EDGE ( 'NONE', *, *, #14261, .F. ) ;
#3884 = DIRECTION ( 'NONE',  ( -0.3747554100459928317, -0.9271237148521548344, 0.000000000000000000 ) ) ;
#3885 = CARTESIAN_POINT ( 'NONE',  ( 97.50000000000002842, -199.9999999999999716, 30.00000000000000000 ) ) ;
#3886 = EDGE_CURVE ( 'NONE', #6696, #10983, #19781, .T. ) ;
#3887 = CARTESIAN_POINT ( 'NONE',  ( 96.48429163929537822, -114.8598460512868513, -9.502487710326173342 ) ) ;
#3888 = FACE_OUTER_BOUND ( 'NONE', #11057, .T. ) ;
#3889 = ORIENTED_EDGE ( 'NONE', *, *, #2310, .T. ) ;
#3890 = EDGE_CURVE ( 'NONE', #16353, #8253, #724, .T. ) ;
#3891 = DIRECTION ( 'NONE',  ( 1.000000000000000000, 0.000000000000000000, 0.000000000000000000 ) ) ;
#3892 = DIRECTION ( 'NONE',  ( 0.2225209339563050392, 0.9749279121818257288, 0.000000000000000000 ) ) ;
#3893 = ORIENTED_EDGE ( 'NONE', *, *, #1097, .T. ) ;
#3894 = ORIENTED_EDGE ( 'NONE', *, *, #9012, .F. ) ;
#3895 = CIRCLE ( 'NONE', #5535, 150.0000000000000284 ) ;
#3896 = AXIS2_PLACEMENT_3D ( 'NONE', #11016, #14092, #15733 ) ;
#3897 = EDGE_CURVE ( 'NONE', #16737, #6676, #19883, .T. ) ;
#3898 = DIRECTION ( 'NONE',  ( 0.000000000000000000, 0.000000000000000000, 1.000000000000000000 ) ) ;
#3899 = EDGE_LOOP ( 'NONE', ( #9673, #1110, #17965, #14978 ) ) ;
#3900 = CARTESIAN_POINT ( 'NONE',  ( 88.01533840461537750, -121.4634816193508300, -4.652272054116179945 ) ) ;
#3901 = CARTESIAN_POINT ( 'NONE',  ( -89.41572940476631004, -120.4415366094358149, -5.961443665946996262 ) ) ;
#3902 = CARTESIAN_POINT ( 'NONE',  ( -82.79607015190578068, -125.0792639210693267, 4.334714214550138500 ) ) ;
#3903 = FACE_OUTER_BOUND ( 'NONE', #11630, .T. ) ;
#3904 = CARTESIAN_POINT ( 'NONE',  ( -1.379293853801755176, 62.90240729679781850, 293.5832628385307999 ) ) ;
#3905 = EDGE_CURVE ( 'NONE', #19703, #6726, #12144, .T. ) ;
#3906 = CARTESIAN_POINT ( 'NONE',  ( 50.37374754117451658, -141.2886604036503115, 60.00000000000000000 ) ) ;
#3907 = CARTESIAN_POINT ( 'NONE',  ( 0.7000608949449850238, 5.693982670708919613, 283.5832628385307999 ) ) ;
#3908 = CIRCLE ( 'NONE', #12714, 112.8770930172170210 ) ;
#3909 = DIRECTION ( 'NONE',  ( 0.000000000000000000, 0.000000000000000000, 1.000000000000000000 ) ) ;
#3910 = VECTOR ( 'NONE', #15811, 1000.000000000000000 ) ;
#3911 = ORIENTED_EDGE ( 'NONE', *, *, #5282, .T. ) ;
#3912 = CARTESIAN_POINT ( 'NONE',  ( -1.607844166819003129E-13, 26.82911281104372847, 14.88498244535545112 ) ) ;
#3913 = DIRECTION ( 'NONE',  ( 1.000000000000000000, 0.000000000000000000, 0.000000000000000000 ) ) ;
#3914 = ADVANCED_FACE ( 'NONE', ( #17786 ), #3666, .T. ) ;
#3915 = VERTEX_POINT ( 'NONE', #9902 ) ;
#3916 = ORIENTED_EDGE ( 'NONE', *, *, #7162, .T. ) ;
#3917 = AXIS2_PLACEMENT_3D ( 'NONE', #13013, #3513, #11386 ) ;
#3918 = ORIENTED_EDGE ( 'NONE', *, *, #19767, .F. ) ;
#3919 = AXIS2_PLACEMENT_3D ( 'NONE', #12195, #9027, #7592 ) ;
#3920 = DIRECTION ( 'NONE',  ( 0.000000000000000000, 0.000000000000000000, -1.000000000000000000 ) ) ;
#3921 = FACE_OUTER_BOUND ( 'NONE', #7832, .T. ) ;
#3922 = LINE ( 'NONE', #3631, #6822 ) ;
#3923 = DIRECTION ( 'NONE',  ( 0.9009688679024221436, -0.4338837391175519032, 0.000000000000000000 ) ) ;
#3924 = CARTESIAN_POINT ( 'NONE',  ( 85.53020504959901871, -140.9188050298377846, 39.99999999999999289 ) ) ;
#3925 = ORIENTED_EDGE ( 'NONE', *, *, #6550, .F. ) ;
#3926 = DIRECTION ( 'NONE',  ( 0.9394263059140722794, -0.3427509529624095941, 0.000000000000000000 ) ) ;
#3927 = CARTESIAN_POINT ( 'NONE',  ( -130.0420013710532601, -74.85033908744654241, 0.7491723846298292688 ) ) ;
#3928 = CARTESIAN_POINT ( 'NONE',  ( 134.7188131035565277, -72.93593548749576883, 9.237785135033714567 ) ) ;
#3929 = DIRECTION ( 'NONE',  ( -0.000000000000000000, -0.000000000000000000, 1.000000000000000000 ) ) ;
#3930 = PLANE ( 'NONE',  #4819 ) ;
#3931 = ORIENTED_EDGE ( 'NONE', *, *, #15757, .T. ) ;
#3932 = VECTOR ( 'NONE', #13276, 1000.000000000000000 ) ;
#3933 = AXIS2_PLACEMENT_3D ( 'NONE', #10022, #16273, #16071 ) ;
#3934 = VERTEX_POINT ( 'NONE', #19222 ) ;
#3935 = VERTEX_POINT ( 'NONE', #11993 ) ;
#3936 = ORIENTED_EDGE ( 'NONE', *, *, #3382, .T. ) ;
#3937 = DIRECTION ( 'NONE',  ( 0.000000000000000000, 0.000000000000000000, 1.000000000000000000 ) ) ;
#3938 = VERTEX_POINT ( 'NONE', #3858 ) ;
#3939 = CYLINDRICAL_SURFACE ( 'NONE', #429, 3.224098631618460331 ) ;
#3940 = VECTOR ( 'NONE', #18791, 1000.000000000000000 ) ;
#3941 = PLANE ( 'NONE',  #5375 ) ;
#3942 = DIRECTION ( 'NONE',  ( 1.000000000000000000, 0.000000000000000000, 0.000000000000000000 ) ) ;
#3943 = EDGE_LOOP ( 'NONE', ( #16570, #18568, #12997, #19890 ) ) ;
#3944 = CIRCLE ( 'NONE', #19631, 9.999999999999994671 ) ;
#3945 = DIRECTION ( 'NONE',  ( -6.982962677686266711E-15, 0.000000000000000000, -1.000000000000000000 ) ) ;
#3946 = CARTESIAN_POINT ( 'NONE',  ( 0.000000000000000000, 0.000000000000000000, 293.5832628385307999 ) ) ;
#3947 = ORIENTED_EDGE ( 'NONE', *, *, #14850, .F. ) ;
#3948 = CARTESIAN_POINT ( 'NONE',  ( 9.381844291199747943, -57.94128254008187184, 248.9926560891072143 ) ) ;
#3949 = LINE ( 'NONE', #16446, #13934 ) ;
#3950 = LINE ( 'NONE', #8657, #17627 ) ;
#3951 = DIRECTION ( 'NONE',  ( -0.8660254037844432595, 0.4999999999999919509, 0.000000000000000000 ) ) ;
#3952 = CIRCLE ( 'NONE', #7227, 150.0000000000000284 ) ;
#3953 = CARTESIAN_POINT ( 'NONE',  ( -140.5398538968364051, -20.43888546547794505, -12.13436485393500419 ) ) ;
#3954 = DIRECTION ( 'NONE',  ( -0.7660444431189770143, 0.6427876096865405842, 5.348151281215662765E-15 ) ) ;
#3955 = ORIENTED_EDGE ( 'NONE', *, *, #1276, .F. ) ;
#3956 = EDGE_CURVE ( 'NONE', #6905, #2638, #16149, .T. ) ;
#3957 = VECTOR ( 'NONE', #202, 999.9999999999998863 ) ;
#3958 = LINE ( 'NONE', #8469, #17102 ) ;
#3959 = ORIENTED_EDGE ( 'NONE', *, *, #5121, .T. ) ;
#3960 = EDGE_LOOP ( 'NONE', ( #7313, #3816, #17135, #10126 ) ) ;
#3961 = CARTESIAN_POINT ( 'NONE',  ( 14.85701326357424890, 22.71800723006102274, 39.88498244535534809 ) ) ;
#3962 = ORIENTED_EDGE ( 'NONE', *, *, #11279, .T. ) ;
#3963 = DIRECTION ( 'NONE',  ( -0.000000000000000000, -0.000000000000000000, -1.000000000000000000 ) ) ;
#3964 = EDGE_CURVE ( 'NONE', #15086, #15546, #10460, .T. ) ;
#3965 = DIRECTION ( 'NONE',  ( 1.000000000000000000, 0.000000000000000000, 0.000000000000000000 ) ) ;
#3966 = CARTESIAN_POINT ( 'NONE',  ( 0.000000000000000000, 0.000000000000000000, -105.0000000000000142 ) ) ;
#3967 = FACE_OUTER_BOUND ( 'NONE', #15282, .T. ) ;
#3968 = EDGE_CURVE ( 'NONE', #9705, #10158, #3988, .T. ) ;
#3969 = ORIENTED_EDGE ( 'NONE', *, *, #3602, .T. ) ;
#3970 = CARTESIAN_POINT ( 'NONE',  ( -134.2425157119612891, -66.92593549375912687, 37.65294690872419636 ) ) ;
#3971 = LINE ( 'NONE', #3775, #1266 ) ;
#3972 = CARTESIAN_POINT ( 'NONE',  ( 0.000000000000000000, 0.000000000000000000, 83.57543755549745867 ) ) ;
#3973 = DIRECTION ( 'NONE',  ( 1.000000000000000000, 0.000000000000000000, 0.000000000000000000 ) ) ;
#3974 = ORIENTED_EDGE ( 'NONE', *, *, #10634, .F. ) ;
#3975 = VECTOR ( 'NONE', #17755, 1000.000000000000000 ) ;
#3976 = DIRECTION ( 'NONE',  ( 0.9781142164131917394, -0.2080686897406911207, 0.000000000000000000 ) ) ;
#3977 = CARTESIAN_POINT ( 'NONE',  ( 84.48076729319797096, -123.9477347680102497, 0.1101890534364035890 ) ) ;
#3978 = CYLINDRICAL_SURFACE ( 'NONE', #9888, 7.500000000000006217 ) ;
#3979 = ORIENTED_EDGE ( 'NONE', *, *, #18502, .F. ) ;
#3980 = EDGE_CURVE ( 'NONE', #2942, #6926, #589, .T. ) ;
#3981 = DIRECTION ( 'NONE',  ( 1.000000000000000000, 0.000000000000000000, 0.000000000000000000 ) ) ;
#3982 = LINE ( 'NONE', #5332, #13486 ) ;
#3983 = ORIENTED_EDGE ( 'NONE', *, *, #12666, .T. ) ;
#3984 = ORIENTED_EDGE ( 'NONE', *, *, #11842, .T. ) ;
#3985 = LINE ( 'NONE', #4396, #16329 ) ;
#3986 = EDGE_CURVE ( 'NONE', #7913, #1086, #8362, .T. ) ;
#3987 = DIRECTION ( 'NONE',  ( 0.000000000000000000, 0.000000000000000000, 1.000000000000000000 ) ) ;
#3988 = CIRCLE ( 'NONE', #5320, 62.91752772691707207 ) ;
#3989 = ORIENTED_EDGE ( 'NONE', *, *, #19494, .T. ) ;
#3990 = CIRCLE ( 'NONE', #6625, 62.91752772691707207 ) ;
#3991 = EDGE_CURVE ( 'NONE', #19110, #16155, #8565, .T. ) ;
#3992 = CARTESIAN_POINT ( 'NONE',  ( 7.950000000000000178, 5.196152422706624030, -9.000000000000001776 ) ) ;
#3993 = CARTESIAN_POINT ( 'NONE',  ( -86.68385341649090492, -122.4206889339686484, -3.257968381067569474 ) ) ;
#3994 = EDGE_CURVE ( 'NONE', #15308, #11944, #13635, .T. ) ;
#3995 = VECTOR ( 'NONE', #10533, 1000.000000000000000 ) ;
#3996 = AXIS2_PLACEMENT_3D ( 'NONE', #19556, #11767, #8709 ) ;
#3997 = CARTESIAN_POINT ( 'NONE',  ( 167.4599531637113330, -36.50981547336952104, 49.99999999999999289 ) ) ;
#3998 = DIRECTION ( 'NONE',  ( 0.9396926207859112035, 0.3420201433256609969, -6.456589605409174593E-15 ) ) ;
#3999 = FACE_OUTER_BOUND ( 'NONE', #1297, .T. ) ;
#4000 = LINE ( 'NONE', #7082, #331 ) ;
#4001 = CARTESIAN_POINT ( 'NONE',  ( -1.289614712049157230, 5.590028426173801357, 293.5832628385307999 ) ) ;
#4002 = CARTESIAN_POINT ( 'NONE',  ( -22.28973221005119854, -58.83691981461626597, 248.9926560891072143 ) ) ;
#4003 = ORIENTED_EDGE ( 'NONE', *, *, #8639, .T. ) ;
#4004 = EDGE_CURVE ( 'NONE', #270, #19664, #12961, .T. ) ;
#4005 = CARTESIAN_POINT ( 'NONE',  ( 0.000000000000000000, 0.000000000000000000, 0.000000000000000000 ) ) ;
#4006 = DIRECTION ( 'NONE',  ( 0.3427509529624096496, 0.9394263059140723904, 0.000000000000000000 ) ) ;
#4007 = VECTOR ( 'NONE', #14949, 1000.000000000000000 ) ;
#4008 = VECTOR ( 'NONE', #576, 999.9999999999998863 ) ;
#4009 = ADVANCED_FACE ( 'NONE', ( #17693, #2136 ), #1160, .T. ) ;
#4010 = EDGE_LOOP ( 'NONE', ( #768, #5381, #14928, #5925 ) ) ;
#4011 = VECTOR ( 'NONE', #15006, 1000.000000000000114 ) ;
#4012 = ORIENTED_EDGE ( 'NONE', *, *, #1615, .F. ) ;
#4013 = DIRECTION ( 'NONE',  ( 0.000000000000000000, 0.000000000000000000, 1.000000000000000000 ) ) ;
#4014 = ORIENTED_EDGE ( 'NONE', *, *, #17032, .F. ) ;
#4015 = ADVANCED_FACE ( 'NONE', ( #3566 ), #9799, .F. ) ;
#4016 = EDGE_CURVE ( 'NONE', #5755, #13097, #6935, .T. ) ;
#4017 = CARTESIAN_POINT ( 'NONE',  ( 134.7188131032333445, -72.93593548660993520, 30.00000000000000000 ) ) ;
#4018 = EDGE_CURVE ( 'NONE', #14124, #3199, #4439, .T. ) ;
#4019 = CARTESIAN_POINT ( 'NONE',  ( -14.69786621328411869, 22.52834316112731017, 14.88498244535555592 ) ) ;
#4020 = AXIS2_PLACEMENT_3D ( 'NONE', #4810, #7861, #9507 ) ;
#4021 = DIRECTION ( 'NONE',  ( -0.000000000000000000, -0.000000000000000000, 1.000000000000000000 ) ) ;
#4022 = VECTOR ( 'NONE', #5055, 1000.000000000000000 ) ;
#4023 = DIRECTION ( 'NONE',  ( 0.000000000000000000, 0.000000000000000000, 1.000000000000000000 ) ) ;
#4024 = ORIENTED_EDGE ( 'NONE', *, *, #19114, .T. ) ;
#4025 = CARTESIAN_POINT ( 'NONE',  ( -26.42151830275515323, 4.658826548058537576, 14.88498244535563586 ) ) ;
#4026 = CARTESIAN_POINT ( 'NONE',  ( -124.9958490024057198, -82.94424249022438289, -0.9643169688603490108 ) ) ;
#4027 = CARTESIAN_POINT ( 'NONE',  ( 22.28973221005080774, 58.83691981461640097, 293.5832628385307999 ) ) ;
#4028 = AXIS2_PLACEMENT_3D ( 'NONE', #17970, #3937, #16432 ) ;
#4029 = DIRECTION ( 'NONE',  ( -1.000000000000000000, 0.000000000000000000, 0.000000000000000000 ) ) ;
#4030 = FACE_OUTER_BOUND ( 'NONE', #13227, .T. ) ;
#4031 = DIRECTION ( 'NONE',  ( -0.000000000000000000, -0.000000000000000000, -1.000000000000000000 ) ) ;
#4032 = ORIENTED_EDGE ( 'NONE', *, *, #9117, .F. ) ;
#4033 = EDGE_CURVE ( 'NONE', #7965, #14351, #3117, .T. ) ;
#4034 = VECTOR ( 'NONE', #8893, 1000.000000000000000 ) ;
#4035 = ORIENTED_EDGE ( 'NONE', *, *, #18390, .T. ) ;
#4036 = ORIENTED_EDGE ( 'NONE', *, *, #8219, .F. ) ;
#4037 = ORIENTED_EDGE ( 'NONE', *, *, #7146, .F. ) ;
#4038 = VERTEX_POINT ( 'NONE', #1269 ) ;
#4039 = EDGE_CURVE ( 'NONE', #19664, #12482, #11515, .T. ) ;
#4040 = AXIS2_PLACEMENT_3D ( 'NONE', #15889, #17535, #19357 ) ;
#4041 = DIRECTION ( 'NONE',  ( 1.224646799147353207E-16, 1.000000000000000000, -0.000000000000000000 ) ) ;
#4042 = CARTESIAN_POINT ( 'NONE',  ( -11.00103590902911499, -57.65577537092155325, 132.4711112102474146 ) ) ;
#4043 = CIRCLE ( 'NONE', #13845, 9.000000000000001776 ) ;
#4044 = CARTESIAN_POINT ( 'NONE',  ( 7.350000000000000533, 5.196152422706624030, -9.000000000000001776 ) ) ;
#4045 = ORIENTED_EDGE ( 'NONE', *, *, #16863, .F. ) ;
#4046 = CARTESIAN_POINT ( 'NONE',  ( -67.50000000000000000, -2.085703952312275003E-13, -105.0000000000000142 ) ) ;
#4047 = CARTESIAN_POINT ( 'NONE',  ( -110.0000000000000142, 265.0000000000000000, 5.000000000000000888 ) ) ;
#4048 = EDGE_CURVE ( 'NONE', #19359, #12474, #9036, .T. ) ;
#4049 = ORIENTED_EDGE ( 'NONE', *, *, #18884, .T. ) ;
#4050 = CARTESIAN_POINT ( 'NONE',  ( 181.0783081749256951, -199.9999999999999716, 40.00000000000000000 ) ) ;
#4051 = CARTESIAN_POINT ( 'NONE',  ( 0.000000000000000000, 0.000000000000000000, 283.5832628385307999 ) ) ;
#4052 = LINE ( 'NONE', #15089, #7479 ) ;
#4053 = DIRECTION ( 'NONE',  ( 0.000000000000000000, 0.000000000000000000, 1.000000000000000000 ) ) ;
#4054 = LINE ( 'NONE', #12224, #11364 ) ;
#4055 = CARTESIAN_POINT ( 'NONE',  ( 36.99387960884163817, -48.17797692984175484, 283.5832628385307999 ) ) ;
#4056 = ORIENTED_EDGE ( 'NONE', *, *, #17125, .T. ) ;
#4057 = DIRECTION ( 'NONE',  ( 0.000000000000000000, 0.000000000000000000, 1.000000000000000000 ) ) ;
#4058 = VECTOR ( 'NONE', #19688, 1000.000000000000000 ) ;
#4059 = EDGE_LOOP ( 'NONE', ( #14370, #6915 ) ) ;
#4060 = ORIENTED_EDGE ( 'NONE', *, *, #12257, .T. ) ;
#4061 = CARTESIAN_POINT ( 'NONE',  ( -19.23614321207234923, 57.61627707419557254, 293.5832628385307999 ) ) ;
#4062 = VERTEX_POINT ( 'NONE', #1578 ) ;
#4063 = EDGE_LOOP ( 'NONE', ( #7211, #1058, #12343 ) ) ;
#4064 = DIRECTION ( 'NONE',  ( 1.000000000000000000, 0.000000000000000000, 0.000000000000000000 ) ) ;
#4065 = CARTESIAN_POINT ( 'NONE',  ( -84.01517049618257715, -124.2637720100346002, 38.96058320792450047 ) ) ;
#4066 = LINE ( 'NONE', #18189, #14871 ) ;
#4067 = DIRECTION ( 'NONE',  ( 0.000000000000000000, 0.000000000000000000, 1.000000000000000000 ) ) ;
#4068 = EDGE_CURVE ( 'NONE', #7735, #7403, #1379, .T. ) ;
#4069 = ORIENTED_EDGE ( 'NONE', *, *, #5286, .F. ) ;
#4070 = DIRECTION ( 'NONE',  ( -0.7406645559057083439, 0.6718749999999998890, 0.000000000000000000 ) ) ;
#4071 = DIRECTION ( 'NONE',  ( 0.000000000000000000, 0.000000000000000000, 1.000000000000000000 ) ) ;
#4072 = CARTESIAN_POINT ( 'NONE',  ( 0.000000000000000000, 0.000000000000000000, 283.5832628385307999 ) ) ;
#4073 = DIRECTION ( 'NONE',  ( -1.000000000000000000, 0.000000000000000000, 0.000000000000000000 ) ) ;
#4074 = ORIENTED_EDGE ( 'NONE', *, *, #5640, .F. ) ;
#4075 = CARTESIAN_POINT ( 'NONE',  ( -110.0000000000000142, 275.0000000000000568, 5.000000000000000888 ) ) ;
#4076 = CARTESIAN_POINT ( 'NONE',  ( 84.01517049618261979, -124.2637720100345717, 1.039416792075506635 ) ) ;
#4077 = AXIS2_PLACEMENT_3D ( 'NONE', #5609, #16753, #13367 ) ;
#4078 = FACE_OUTER_BOUND ( 'NONE', #988, .T. ) ;
#4079 = ORIENTED_EDGE ( 'NONE', *, *, #547, .T. ) ;
#4080 = EDGE_CURVE ( 'NONE', #4164, #13913, #14132, .T. ) ;
#4081 = DIRECTION ( 'NONE',  ( 0.7430374143461900838, -0.6692498792541753394, 0.000000000000000000 ) ) ;
#4082 = DIRECTION ( 'NONE',  ( 0.000000000000000000, 0.000000000000000000, 1.000000000000000000 ) ) ;
#4083 = ORIENTED_EDGE ( 'NONE', *, *, #13614, .F. ) ;
#4084 = AXIS2_PLACEMENT_3D ( 'NONE', #19276, #11584, #14458 ) ;
#4085 = ORIENTED_EDGE ( 'NONE', *, *, #388, .T. ) ;
#4086 = ORIENTED_EDGE ( 'NONE', *, *, #1535, .T. ) ;
#4087 = CARTESIAN_POINT ( 'NONE',  ( -21.73104181959847025, -16.26654594725001957, 14.88498244535560389 ) ) ;
#4088 = DIRECTION ( 'NONE',  ( 0.000000000000000000, 0.000000000000000000, -1.000000000000000000 ) ) ;
#4089 = ORIENTED_EDGE ( 'NONE', *, *, #16386, .T. ) ;
#4090 = AXIS2_PLACEMENT_3D ( 'NONE', #17899, #17997, #19434 ) ;
#4091 = CARTESIAN_POINT ( 'NONE',  ( 98.69083902877214598, -112.9691409624333573, -9.907675691193132295 ) ) ;
#4092 = DIRECTION ( 'NONE',  ( -0.000000000000000000, -0.000000000000000000, -1.000000000000000000 ) ) ;
#4093 = EDGE_CURVE ( 'NONE', #301, #18014, #1683, .T. ) ;
#4094 = EDGE_CURVE ( 'NONE', #9575, #14124, #9349, .T. ) ;
#4095 = DIRECTION ( 'NONE',  ( 0.9902903945359623483, 0.1390141521205945918, 0.000000000000000000 ) ) ;
#4096 = PLANE ( 'NONE',  #5596 ) ;
#4097 = DIRECTION ( 'NONE',  ( -0.4999999999999919509, -0.8660254037844432595, 0.000000000000000000 ) ) ;
#4098 = DIRECTION ( 'NONE',  ( 1.000000000000000000, 0.000000000000000000, 0.000000000000000000 ) ) ;
#4099 = SHAPE_REPRESENTATION_RELATIONSHIP ( 'NONE' , 'NONE' ,  #2084, #13837 ) ;
#4100 = DIRECTION ( 'NONE',  ( -0.7430374143461878633, 0.6692498792541777819, 0.000000000000000000 ) ) ;
#4101 = DIRECTION ( 'NONE',  ( 6.982962677686266711E-15, -0.000000000000000000, 1.000000000000000000 ) ) ;
#4102 = CIRCLE ( 'NONE', #13902, 10.00000000000000888 ) ;
#4103 = VERTEX_POINT ( 'NONE', #9247 ) ;
#4104 = ADVANCED_FACE ( 'NONE', ( #13740 ), #10777, .F. ) ;
#4105 = DIRECTION ( 'NONE',  ( -0.000000000000000000, 0.5000000000000012212, 0.8660254037844379305 ) ) ;
#4106 = CYLINDRICAL_SURFACE ( 'NONE', #3698, 9.999999999999994671 ) ;
#4107 = ADVANCED_FACE ( 'NONE', ( #19982 ), #13844, .T. ) ;
#4108 = VERTEX_POINT ( 'NONE', #14055 ) ;
#4109 = EDGE_CURVE ( 'NONE', #18597, #4682, #1475, .T. ) ;
#4110 = ORIENTED_EDGE ( 'NONE', *, *, #18588, .F. ) ;
#4111 = ORIENTED_EDGE ( 'NONE', *, *, #18557, .T. ) ;
#4112 = CARTESIAN_POINT ( 'NONE',  ( 22.28973221005081129, 58.83691981461641518, 132.4711112102474146 ) ) ;
#4113 = ORIENTED_EDGE ( 'NONE', *, *, #5371, .F. ) ;
#4114 = CARTESIAN_POINT ( 'NONE',  ( -97.77191798235051579, 62.82820655979934088, 14.88498244535613502 ) ) ;
#4115 = LINE ( 'NONE', #4316, #17284 ) ;
#4116 = AXIS2_PLACEMENT_3D ( 'NONE', #15583, #9446, #12601 ) ;
#4117 = EDGE_CURVE ( 'NONE', #18256, #7769, #6196, .T. ) ;
#4118 = EDGE_CURVE ( 'NONE', #16923, #16598, #15430, .T. ) ;
#4119 = DIRECTION ( 'NONE',  ( -0.9848077530122091305, 0.1736481776669241417, 0.000000000000000000 ) ) ;
#4120 = CARTESIAN_POINT ( 'NONE',  ( -98.69083902876617742, -112.9691409624384733, 49.90767569119055480 ) ) ;
#4121 = DIRECTION ( 'NONE',  ( 0.000000000000000000, 0.000000000000000000, -1.000000000000000000 ) ) ;
#4122 = ORIENTED_EDGE ( 'NONE', *, *, #5532, .T. ) ;
#4123 = DIRECTION ( 'NONE',  ( 0.3427509529624101492, -0.9394263059140720573, -0.000000000000000000 ) ) ;
#4124 = CARTESIAN_POINT ( 'NONE',  ( -132.2990932590211628, -86.73761849284356629, 0.4401276754358985355 ) ) ;
#4125 = CIRCLE ( 'NONE', #13924, 27.50000000000000355 ) ;
#4126 = CARTESIAN_POINT ( 'NONE',  ( 134.5311723999374465, -74.37598470587731470, 6.383662503987586945 ) ) ;
#4127 = CARTESIAN_POINT ( 'NONE',  ( 0.000000000000000000, 0.000000000000000000, 293.5832628385307999 ) ) ;
#4128 = DIRECTION ( 'NONE',  ( -0.000000000000000000, -0.000000000000000000, 1.000000000000000000 ) ) ;
#4129 = DIRECTION ( 'NONE',  ( 0.000000000000000000, 0.000000000000000000, 1.000000000000000000 ) ) ;
#4130 = ADVANCED_FACE ( 'NONE', ( #1372 ), #6296, .F. ) ;
#4132 = EDGE_CURVE ( 'NONE', #18385, #10900, #19371, .T. ) ;
#4131 = AXIS2_PLACEMENT_3D ( 'NONE', #10121, #8972, #18193 ) ;
#4133 = ADVANCED_FACE ( 'NONE', ( #5983 ), #20086, .T. ) ;
#4134 = PRODUCT_RELATED_PRODUCT_CATEGORY ( 'part', '', ( #1811 ) ) ;
#4135 = EDGE_LOOP ( 'NONE', ( #14885, #12306, #9777 ) ) ;
#4136 = AXIS2_PLACEMENT_3D ( 'NONE', #1865, #6684, #8200 ) ;
#4137 = ADVANCED_FACE ( 'NONE', ( #6395 ), #7601, .T. ) ;
#4138 = ORIENTED_EDGE ( 'NONE', *, *, #11663, .T. ) ;
#4139 = VERTEX_POINT ( 'NONE', #11081 ) ;
#4140 = AXIS2_PLACEMENT_3D ( 'NONE', #2879, #13604, #9106 ) ;
#4141 = ORIENTED_EDGE ( 'NONE', *, *, #14238, .T. ) ;
#4142 = EDGE_CURVE ( 'NONE', #3424, #15773, #16334, .T. ) ;
#4143 = FACE_OUTER_BOUND ( 'NONE', #16593, .T. ) ;
#4144 = CARTESIAN_POINT ( 'NONE',  ( 0.000000000000000000, 0.000000000000000000, 283.5832628385307999 ) ) ;
#4145 = ORIENTED_EDGE ( 'NONE', *, *, #7409, .F. ) ;
#4146 = CARTESIAN_POINT ( 'NONE',  ( -1.148576676476831260E-14, -8.236864015571811137, 3.733333029993802565 ) ) ;
#4147 = CARTESIAN_POINT ( 'NONE',  ( 0.000000000000000000, 0.000000000000000000, 293.5832628385307999 ) ) ;
#4148 = ORIENTED_EDGE ( 'NONE', *, *, #6993, .F. ) ;
#4149 = DIRECTION ( 'NONE',  ( -1.000000000000000000, -0.000000000000000000, -0.000000000000000000 ) ) ;
#4150 = DIRECTION ( 'NONE',  ( -0.3747554100459928317, -0.9271237148521548344, 0.000000000000000000 ) ) ;
#4151 = CARTESIAN_POINT ( 'NONE',  ( -133.1916981995337892, -82.53555109165357351, 1.486209767972074047 ) ) ;
#4152 = DIRECTION ( 'NONE',  ( -0.000000000000000000, -0.000000000000000000, 1.000000000000000000 ) ) ;
#4153 = CIRCLE ( 'NONE', #10688, 7.500000000000006217 ) ;
#4154 = EDGE_CURVE ( 'NONE', #6500, #12180, #8113, .T. ) ;
#4155 = EDGE_CURVE ( 'NONE', #10080, #3915, #10520, .T. ) ;
#4156 = DIRECTION ( 'NONE',  ( 0.000000000000000000, 0.000000000000000000, 1.000000000000000000 ) ) ;
#4157 = CARTESIAN_POINT ( 'NONE',  ( -23.23469325536255070, -13.41455640552162443, 39.88498244535561810 ) ) ;
#4158 = ORIENTED_EDGE ( 'NONE', *, *, #9916, .F. ) ;
#4159 = CARTESIAN_POINT ( 'NONE',  ( 0.000000000000000000, 0.000000000000000000, 0.000000000000000000 ) ) ;
#4160 = ORIENTED_EDGE ( 'NONE', *, *, #11040, .T. ) ;
#4161 = EDGE_CURVE ( 'NONE', #19269, #13184, #6797, .T. ) ;
#4162 = ORIENTED_EDGE ( 'NONE', *, *, #14879, .F. ) ;
#4163 = CARTESIAN_POINT ( 'NONE',  ( -65.74260934110282051, 0.000000000000000000, 293.5832628385307999 ) ) ;
#4164 = VERTEX_POINT ( 'NONE', #14565 ) ;
#4165 = ORIENTED_EDGE ( 'NONE', *, *, #17691, .F. ) ;
#4166 = VECTOR ( 'NONE', #10347, 1000.000000000000000 ) ;
#4167 = DIRECTION ( 'NONE',  ( -0.8660254037844415942, 0.4999999999999950040, 0.000000000000000000 ) ) ;
#4168 = VECTOR ( 'NONE', #13921, 1000.000000000000000 ) ;
#4169 = LINE ( 'NONE', #16852, #127 ) ;
#4170 = DIRECTION ( 'NONE',  ( 1.000000000000000000, 0.000000000000000000, 0.000000000000000000 ) ) ;
#4171 = DIRECTION ( 'NONE',  ( -0.000000000000000000, 1.000000000000000000, 0.000000000000000000 ) ) ;
#4172 = CYLINDRICAL_SURFACE ( 'NONE', #11904, 7.500000000000001776 ) ;
#4173 = ORIENTED_EDGE ( 'NONE', *, *, #4760, .T. ) ;
#4174 = CARTESIAN_POINT ( 'NONE',  ( -125.6254798881099362, -81.96796683352710033, 49.52966944193529741 ) ) ;
#4175 = DIRECTION ( 'NONE',  ( 0.6427876096865379196, 0.7660444431189792347, 0.000000000000000000 ) ) ;
#4176 = FACE_OUTER_BOUND ( 'NONE', #8033, .T. ) ;
#4177 = EDGE_LOOP ( 'NONE', ( #15426, #3594, #10500, #9250 ) ) ;
#4178 = DIRECTION ( 'NONE',  ( 0.1736481776669374366, -0.9848077530122066880, 0.000000000000000000 ) ) ;
#4179 = CARTESIAN_POINT ( 'NONE',  ( -148.9554720520392834, -17.67108784863416560, 39.99999999999999289 ) ) ;
#4180 = FACE_OUTER_BOUND ( 'NONE', #12731, .T. ) ;
#4181 = AXIS2_PLACEMENT_3D ( 'NONE', #16932, #15288, #2922 ) ;
#4182 = VERTEX_POINT ( 'NONE', #9556 ) ;
#4183 = AXIS2_PLACEMENT_3D ( 'NONE', #16892, #9107, #208 ) ;
#4184 = CIRCLE ( 'NONE', #927, 60.74260934110282051 ) ;
#4185 = DIRECTION ( 'NONE',  ( 0.000000000000000000, 0.000000000000000000, 1.000000000000000000 ) ) ;
#4186 = DIRECTION ( 'NONE',  ( -1.000000000000000000, 0.000000000000000000, -0.000000000000000000 ) ) ;
#4187 = ORIENTED_EDGE ( 'NONE', *, *, #9409, .T. ) ;
#4188 = VERTEX_POINT ( 'NONE', #554 ) ;
#4189 = CARTESIAN_POINT ( 'NONE',  ( 79.75827554147308263, 0.000000000000000000, 293.5832628385307999 ) ) ;
#4190 = ORIENTED_EDGE ( 'NONE', *, *, #14549, .F. ) ;
#4191 = CARTESIAN_POINT ( 'NONE',  ( -79.05640494597940915, -127.4758205975444270, 49.99999999999999289 ) ) ;
#4192 = DIRECTION ( 'NONE',  ( 1.000000000000000000, 0.000000000000000000, 0.000000000000000000 ) ) ;
#4193 = VERTEX_POINT ( 'NONE', #13018 ) ;
#4194 = VECTOR ( 'NONE', #3871, 1000.000000000000000 ) ;
#4195 = CYLINDRICAL_SURFACE ( 'NONE', #8994, 60.74260934110282051 ) ;
#4196 = CARTESIAN_POINT ( 'NONE',  ( 118.3534152657848608, 114.7431683447366595, 39.99999999999999289 ) ) ;
#4197 = CIRCLE ( 'NONE', #925, 17.50000000000001066 ) ;
#4198 = AXIS2_PLACEMENT_3D ( 'NONE', #903, #10404, #5613 ) ;
#4199 = CIRCLE ( 'NONE', #2260, 7.500000000000001776 ) ;
#4200 = LINE ( 'NONE', #18922, #13421 ) ;
#4201 = LINE ( 'NONE', #1126, #17785 ) ;
#4202 = FACE_BOUND ( 'NONE', #16039, .T. ) ;
#4203 = CYLINDRICAL_SURFACE ( 'NONE', #18192, 150.0000000000000284 ) ;
#4204 = FACE_OUTER_BOUND ( 'NONE', #10436, .T. ) ;
#4205 = DIRECTION ( 'NONE',  ( 0.000000000000000000, 0.000000000000000000, -1.000000000000000000 ) ) ;
#4206 = EDGE_LOOP ( 'NONE', ( #3848, #19881, #18876, #2939, #7895 ) ) ;
#4207 = FACE_OUTER_BOUND ( 'NONE', #11898, .T. ) ;
#4208 = CARTESIAN_POINT ( 'NONE',  ( 58.03804081968166173, -8.833100819207778898, 132.4711112102474146 ) ) ;
#4209 = ORIENTED_EDGE ( 'NONE', *, *, #11907, .F. ) ;
#4210 = AXIS2_PLACEMENT_3D ( 'NONE', #14405, #7030, #783 ) ;
#4211 = AXIS2_PLACEMENT_3D ( 'NONE', #11120, #12448, #8050 ) ;
#4212 = EDGE_CURVE ( 'NONE', #15168, #2215, #19279, .T. ) ;
#4213 = ORIENTED_EDGE ( 'NONE', *, *, #2607, .F. ) ;
#4214 = ORIENTED_EDGE ( 'NONE', *, *, #11535, .T. ) ;
#4215 = LINE ( 'NONE', #11321, #3492 ) ;
#4216 = VERTEX_POINT ( 'NONE', #17736 ) ;
#4217 = CARTESIAN_POINT ( 'NONE',  ( 134.0425641885189805, -77.70550467234687630, 3.648054164520854847 ) ) ;
#4218 = CARTESIAN_POINT ( 'NONE',  ( 12.50000000000006750, 0.000000000000000000, 0.000000000000000000 ) ) ;
#4219 = CARTESIAN_POINT ( 'NONE',  ( 12.23146955673593794, 77.31114765718498916, 112.0427633081292953 ) ) ;
#4220 = EDGE_CURVE ( 'NONE', #6267, #8471, #5633, .T. ) ;
#4221 = PLANE ( 'NONE',  #7792 ) ;
#4222 = EDGE_CURVE ( 'NONE', #3408, #1238, #1783, .T. ) ;
#4223 = DIRECTION ( 'NONE',  ( 1.000000000000000000, 3.491481338843133355E-15, 0.000000000000000000 ) ) ;
#4224 = AXIS2_PLACEMENT_3D ( 'NONE', #16878, #18420, #7360 ) ;
#4225 = VECTOR ( 'NONE', #17458, 1000.000000000000000 ) ;
#4226 = EDGE_LOOP ( 'NONE', ( #3170, #17495, #18799, #18677 ) ) ;
#4227 = EDGE_CURVE ( 'NONE', #15975, #14511, #3517, .T. ) ;
#4228 = DIRECTION ( 'NONE',  ( -0.1736481776669374366, 0.9848077530122067991, 0.000000000000000000 ) ) ;
#4229 = CARTESIAN_POINT ( 'NONE',  ( -134.2531151303053036, -76.34772591580372136, 4.523541615885667611 ) ) ;
#4230 = CARTESIAN_POINT ( 'NONE',  ( 76.83212392882491315, 14.94814811854987191, 248.9926560891072143 ) ) ;
#4231 = CARTESIAN_POINT ( 'NONE',  ( -174.2942412179009466, -197.9050378206823098, 1.885337547879245069E-14 ) ) ;
#4232 = DIRECTION ( 'NONE',  ( 0.000000000000000000, 0.000000000000000000, 1.000000000000000000 ) ) ;
#4233 = CARTESIAN_POINT ( 'NONE',  ( 97.50000000000002842, -189.9999999999999716, 30.00000000000000000 ) ) ;
#4234 = VERTEX_POINT ( 'NONE', #9956 ) ;
#4235 = CARTESIAN_POINT ( 'NONE',  ( -78.68887634719368407, -147.8252249328922687, 60.00000000000000000 ) ) ;
#4236 = ADVANCED_FACE ( 'NONE', ( #16005 ), #6495, .F. ) ;
#4237 = EDGE_LOOP ( 'NONE', ( #3576, #1587, #7166 ) ) ;
#4238 = ORIENTED_EDGE ( 'NONE', *, *, #1732, .T. ) ;
#4239 = EDGE_LOOP ( 'NONE', ( #6061, #14587, #19473, #19974 ) ) ;
#4240 = ORIENTED_EDGE ( 'NONE', *, *, #11221, .T. ) ;
#4241 = CARTESIAN_POINT ( 'NONE',  ( 135.7779226595531270, 102.2982297021113141, 60.00000000000000000 ) ) ;
#4242 = EDGE_CURVE ( 'NONE', #141, #19127, #11182, .T. ) ;
#4243 = ORIENTED_EDGE ( 'NONE', *, *, #14284, .F. ) ;
#4244 = EDGE_CURVE ( 'NONE', #11053, #269, #2055, .T. ) ;
#4245 = DIRECTION ( 'NONE',  ( -0.000000000000000000, -0.000000000000000000, 1.000000000000000000 ) ) ;
#4246 = DIRECTION ( 'NONE',  ( 0.9848077530122073542, 0.1736481776669340227, 0.000000000000000000 ) ) ;
#4247 = EDGE_CURVE ( 'NONE', #1319, #3938, #19560, .T. ) ;
#4248 = ORIENTED_EDGE ( 'NONE', *, *, #525, .T. ) ;
#4249 = LINE ( 'NONE', #16244, #17291 ) ;
#4250 = VECTOR ( 'NONE', #4592, 1000.000000000000000 ) ;
#4251 = CARTESIAN_POINT ( 'NONE',  ( 0.000000000000000000, 7.794228634059940930, -4.500000000000011546 ) ) ;
#4252 = CARTESIAN_POINT ( 'NONE',  ( 41.69438488732666315, 106.8146822993833780, 14.88498244535515980 ) ) ;
#4253 = VECTOR ( 'NONE', #16688, 1000.000000000000000 ) ;
#4254 = LINE ( 'NONE', #13658, #13095 ) ;
#4255 = CARTESIAN_POINT ( 'NONE',  ( 27.53920554013639688, 73.25972925305639194, 132.4711112102474146 ) ) ;
#4256 = LINE ( 'NONE', #15195, #1522 ) ;
#4257 = ORIENTED_EDGE ( 'NONE', *, *, #656, .T. ) ;
#4258 = EDGE_CURVE ( 'NONE', #11632, #5887, #16403, .T. ) ;
#4259 = DIRECTION ( 'NONE',  ( -1.000000000000000000, 0.000000000000000000, 7.007922368489490773E-15 ) ) ;
#4260 = ORIENTED_EDGE ( 'NONE', *, *, #14996, .F. ) ;
#4261 = ORIENTED_EDGE ( 'NONE', *, *, #5809, .T. ) ;
#4262 = CARTESIAN_POINT ( 'NONE',  ( 3.911853314815631588, -4.196299268919051251, 283.5832628385307999 ) ) ;
#4263 = AXIS2_PLACEMENT_3D ( 'NONE', #9499, #4404, #11958 ) ;
#4264 = EDGE_LOOP ( 'NONE', ( #4368, #6719, #5070, #9063 ) ) ;
#4265 = VERTEX_POINT ( 'NONE', #17941 ) ;
#4266 = VECTOR ( 'NONE', #13471, 1000.000000000000000 ) ;
#4267 = DIRECTION ( 'NONE',  ( 1.000000000000000000, 0.000000000000000000, 0.000000000000000000 ) ) ;
#4268 = CARTESIAN_POINT ( 'NONE',  ( 30.74413178637192701, -54.89456854707552935, 132.4711112102474146 ) ) ;
#4269 = EDGE_LOOP ( 'NONE', ( #18479, #4086, #361, #1620 ) ) ;
#4270 = EDGE_CURVE ( 'NONE', #2211, #3220, #2383, .T. ) ;
#4271 = CARTESIAN_POINT ( 'NONE',  ( 48.72193424476450474, 39.80940113486034448, 293.5832628385307999 ) ) ;
#4272 = CARTESIAN_POINT ( 'NONE',  ( -59.39925916207560164, -20.74471755083584412, 132.4711112102474146 ) ) ;
#4273 = EDGE_CURVE ( 'NONE', #4648, #5962, #8713, .T. ) ;
#4274 = ORIENTED_EDGE ( 'NONE', *, *, #11719, .T. ) ;
#4275 = DIRECTION ( 'NONE',  ( -0.9396926207859092051, 0.3420201433256662704, 0.000000000000000000 ) ) ;
#4276 = CARTESIAN_POINT ( 'NONE',  ( 32.16802499836741447, 54.07248341783265033, 293.5832628385307999 ) ) ;
#4277 = EDGE_CURVE ( 'NONE', #2619, #6330, #10245, .T. ) ;
#4278 = CARTESIAN_POINT ( 'NONE',  ( 57.65577537092158877, -11.00103590902891249, 132.4711112102474146 ) ) ;
#4279 = AXIS2_PLACEMENT_3D ( 'NONE', #10191, #13349, #11809 ) ;
#4280 = ORIENTED_EDGE ( 'NONE', *, *, #9023, .F. ) ;
#4281 = CARTESIAN_POINT ( 'NONE',  ( 103.2967819461768073, 53.25886146954521649, 14.88498244535472992 ) ) ;
#4282 = PLANE ( 'NONE',  #17345 ) ;
#4283 = CIRCLE ( 'NONE', #14745, 7.500000000000020428 ) ;
#4284 = CARTESIAN_POINT ( 'NONE',  ( -79.51226524016391295, 115.2339015673091041, 22.26257494144193672 ) ) ;
#4285 = EDGE_LOOP ( 'NONE', ( #10270, #13770, #8364, #14184 ) ) ;
#4286 = DIRECTION ( 'NONE',  ( 0.9009688679024221436, -0.4338837391175519032, 0.000000000000000000 ) ) ;
#4287 = DIRECTION ( 'NONE',  ( 0.000000000000000000, 0.000000000000000000, 1.000000000000000000 ) ) ;
#4288 = EDGE_CURVE ( 'NONE', #18107, #5657, #15152, .T. ) ;
#4289 = ORIENTED_EDGE ( 'NONE', *, *, #19302, .T. ) ;
#4290 = ORIENTED_EDGE ( 'NONE', *, *, #8914, .T. ) ;
#4291 = DIRECTION ( 'NONE',  ( 1.000000000000000000, 0.000000000000000000, -0.000000000000000000 ) ) ;
#4292 = ORIENTED_EDGE ( 'NONE', *, *, #7908, .T. ) ;
#4293 = DIRECTION ( 'NONE',  ( 0.000000000000000000, 0.000000000000000000, 1.000000000000000000 ) ) ;
#4294 = CARTESIAN_POINT ( 'NONE',  ( -110.0000000000000142, 285.0000000000000568, 5.000000000000000888 ) ) ;
#4295 = EDGE_LOOP ( 'NONE', ( #9904, #2927, #14343, #12946 ) ) ;
#4296 = CARTESIAN_POINT ( 'NONE',  ( 100.7812500000000284, -111.0996833858562667, -10.00000000000000355 ) ) ;
#4297 = CARTESIAN_POINT ( 'NONE',  ( 0.000000000000000000, 0.000000000000000000, 283.5832628385307999 ) ) ;
#4298 = EDGE_CURVE ( 'NONE', #14566, #15008, #12160, .T. ) ;
#4299 = LINE ( 'NONE', #9103, #8513 ) ;
#4300 = PRESENTATION_STYLE_ASSIGNMENT (( #7468 ) ) ;
#4301 = FACE_BOUND ( 'NONE', #11309, .T. ) ;
#4302 = DIRECTION ( 'NONE',  ( -0.000000000000000000, -0.000000000000000000, 1.000000000000000000 ) ) ;
#4303 = CARTESIAN_POINT ( 'NONE',  ( 4.189777606611760026E-13, -60.00000000000000000, -115.0000000000000000 ) ) ;
#4304 = CARTESIAN_POINT ( 'NONE',  ( -20.84572577951200500, -54.86954475316249358, 248.9926560891072143 ) ) ;
#4305 = EDGE_LOOP ( 'NONE', ( #11207, #9441, #19175, #19401 ) ) ;
#4306 = DIRECTION ( 'NONE',  ( -0.9781142164131917394, 0.2080686897406911207, 0.000000000000000000 ) ) ;
#4307 = LINE ( 'NONE', #9429, #7934 ) ;
#4308 = ORIENTED_EDGE ( 'NONE', *, *, #1629, .T. ) ;
#4309 = ORIENTED_EDGE ( 'NONE', *, *, #6895, .F. ) ;
#4310 = AXIS2_PLACEMENT_3D ( 'NONE', #11501, #10263, #19292 ) ;
#4311 = ORIENTED_EDGE ( 'NONE', *, *, #2510, .F. ) ;
#4312 = FACE_BOUND ( 'NONE', #10602, .T. ) ;
#4313 = ORIENTED_EDGE ( 'NONE', *, *, #12979, .T. ) ;
#4314 = LINE ( 'NONE', #8449, #2397 ) ;
#4315 = CARTESIAN_POINT ( 'NONE',  ( 132.6218665116185207, -85.29503539049812844, 0.7312914155056859933 ) ) ;
#4316 = CARTESIAN_POINT ( 'NONE',  ( -12.78021302872797449, 77.21438937758516374, 112.0427633081291816 ) ) ;
#4317 = CARTESIAN_POINT ( 'NONE',  ( -79.05640494597940915, -127.4758205975444270, 60.00000000000000000 ) ) ;
#4318 = CARTESIAN_POINT ( 'NONE',  ( 0.000000000000000000, 0.000000000000000000, 4.999999999999948486 ) ) ;
#4319 = DIRECTION ( 'NONE',  ( -0.6427876096865300370, -0.7660444431189858960, -0.000000000000000000 ) ) ;
#4320 = EDGE_CURVE ( 'NONE', #12923, #14390, #2682, .T. ) ;
#4321 = ORIENTED_EDGE ( 'NONE', *, *, #5405, .F. ) ;
#4322 = CARTESIAN_POINT ( 'NONE',  ( 28.94886449118905247, -53.40063514825087765, 283.5832628385307999 ) ) ;
#4323 = CARTESIAN_POINT ( 'NONE',  ( -133.0788080491334142, -69.33756331725891187, 7.374420170790281226 ) ) ;
#4324 = CARTESIAN_POINT ( 'NONE',  ( 133.8587666923837105, -78.85012038918880251, 2.995270696459912063 ) ) ;
#4325 = AXIS2_PLACEMENT_3D ( 'NONE', #15176, #6836, #14703 ) ;
#4326 = AXIS2_PLACEMENT_3D ( 'NONE', #17810, #16074, #3780 ) ;
#4327 = FACE_OUTER_BOUND ( 'NONE', #10521, .T. ) ;
#4328 = DIRECTION ( 'NONE',  ( 0.4338837391175509040, 0.9009688679024224767, 0.000000000000000000 ) ) ;
#4329 = CARTESIAN_POINT ( 'NONE',  ( -134.6385828715869479, -73.56429320929808569, 32.40089326748427112 ) ) ;
#4330 = VERTEX_POINT ( 'NONE', #11865 ) ;
#4331 = CARTESIAN_POINT ( 'NONE',  ( -110.0000000000000142, 275.0000000000000000, 5.000000000000000888 ) ) ;
#4332 = AXIS2_PLACEMENT_3D ( 'NONE', #4487, #16973, #13893 ) ;
#4333 = ORIENTED_EDGE ( 'NONE', *, *, #3119, .T. ) ;
#4334 = EDGE_CURVE ( 'NONE', #5779, #17978, #1734, .T. ) ;
#4335 = VERTEX_POINT ( 'NONE', #5552 ) ;
#4336 = ORIENTED_EDGE ( 'NONE', *, *, #3381, .F. ) ;
#4337 = CIRCLE ( 'NONE', #2384, 15.91767397667355510 ) ;
#4338 = AXIS2_PLACEMENT_3D ( 'NONE', #15728, #1709, #14394 ) ;
#4339 = ORIENTED_EDGE ( 'NONE', *, *, #3855, .F. ) ;
#4340 = CARTESIAN_POINT ( 'NONE',  ( -140.6610699913552764, -20.33010010770880172, 21.89506024342324153 ) ) ;
#4341 = CARTESIAN_POINT ( 'NONE',  ( -110.0000000000000142, 165.0000000000000000, 44.99999999999998579 ) ) ;
#4342 = DIRECTION ( 'NONE',  ( -1.000000000000000000, -0.000000000000000000, -0.000000000000000000 ) ) ;
#4343 = ORIENTED_EDGE ( 'NONE', *, *, #18502, .T. ) ;
#4344 = CIRCLE ( 'NONE', #13475, 45.00000000000001421 ) ;
#4345 = DIRECTION ( 'NONE',  ( 0.8186676071302501079, 0.5742676632334704490, -6.938893903907233308E-16 ) ) ;
#4346 = DIRECTION ( 'NONE',  ( 0.000000000000000000, 0.000000000000000000, 1.000000000000000000 ) ) ;
#4347 = EDGE_CURVE ( 'NONE', #4753, #9432, #18036, .T. ) ;
#4348 = VERTEX_POINT ( 'NONE', #3814 ) ;
#4349 = CARTESIAN_POINT ( 'NONE',  ( 0.000000000000000000, 0.000000000000000000, 293.5832628385307999 ) ) ;
#4350 = CARTESIAN_POINT ( 'NONE',  ( -4.581103194068993467, 3.453261854572371892, 283.5832628385307999 ) ) ;
#4351 = CARTESIAN_POINT ( 'NONE',  ( -134.7088667886416999, -73.01552020433989298, 9.022702824945225686 ) ) ;
#4352 = LINE ( 'NONE', #10686, #3940 ) ;
#4353 = UNCERTAINTY_MEASURE_WITH_UNIT (LENGTH_MEASURE( 1.000000000000000082E-05 ), #8097, 'distance_accuracy_value', 'NONE');
#4354 = VECTOR ( 'NONE', #9194, 1000.000000000000114 ) ;
#4355 = CARTESIAN_POINT ( 'NONE',  ( 125.9311142016122034, -81.50627728739362965, 49.44517127269371315 ) ) ;
#4356 = LINE ( 'NONE', #12226, #16879 ) ;
#4357 = EDGE_LOOP ( 'NONE', ( #5872, #7950, #2816, #10174 ) ) ;
#4358 = ORIENTED_EDGE ( 'NONE', *, *, #14102, .F. ) ;
#4359 = EDGE_CURVE ( 'NONE', #1787, #11573, #10059, .T. ) ;
#4360 = DIRECTION ( 'NONE',  ( 0.000000000000000000, 0.000000000000000000, 1.000000000000000000 ) ) ;
#4361 = EDGE_LOOP ( 'NONE', ( #10250, #8749 ) ) ;
#4362 = VECTOR ( 'NONE', #945, 1000.000000000000227 ) ;
#4363 = ORIENTED_EDGE ( 'NONE', *, *, #9279, .T. ) ;
#4364 = EDGE_CURVE ( 'NONE', #315, #17480, #5337, .T. ) ;
#4365 = LINE ( 'NONE', #20014, #758 ) ;
#4366 = VECTOR ( 'NONE', #17401, 1000.000000000000000 ) ;
#4367 = ORIENTED_EDGE ( 'NONE', *, *, #1903, .T. ) ;
#4368 = ORIENTED_EDGE ( 'NONE', *, *, #12488, .T. ) ;
#4369 = CARTESIAN_POINT ( 'NONE',  ( -9.381844291199351815, 57.94128254008192158, 132.4711112102474146 ) ) ;
#4370 =( LENGTH_UNIT ( ) NAMED_UNIT ( * ) SI_UNIT ( .MILLI., .METRE. ) );
#4371 = CARTESIAN_POINT ( 'NONE',  ( 106.6880305650188347, 105.4403344747995988, 49.99999999999999289 ) ) ;
#4372 = VERTEX_POINT ( 'NONE', #10154 ) ;
#4373 = DIRECTION ( 'NONE',  ( 4.650550193362991910E-16, 1.000000000000000000, 0.000000000000000000 ) ) ;
#4374 = CARTESIAN_POINT ( 'NONE',  ( -141.8714406926361562, -48.70825716237266079, 49.99999999999999289 ) ) ;
#4375 = ORIENTED_EDGE ( 'NONE', *, *, #12727, .F. ) ;
#4376 = EDGE_CURVE ( 'NONE', #16627, #3202, #10211, .T. ) ;
#4377 = CARTESIAN_POINT ( 'NONE',  ( 39.80940113486020948, -48.72193424476463974, 132.4711112102474146 ) ) ;
#4378 = CYLINDRICAL_SURFACE ( 'NONE', #11392, 3.224098631618460331 ) ;
#4379 = CIRCLE ( 'NONE', #12210, 9.000000000000000000 ) ;
#4380 = CARTESIAN_POINT ( 'NONE',  ( 25.98398601615827985, 7.853099154550822192, 14.88498244535527171 ) ) ;
#4381 = VECTOR ( 'NONE', #9150, 999.9999999999998863 ) ;
#4382 = DIRECTION ( 'NONE',  ( 6.982962677686266711E-15, -0.000000000000000000, 1.000000000000000000 ) ) ;
#4383 = DIRECTION ( 'NONE',  ( -0.3420201433256630508, -0.9396926207859104263, 0.000000000000000000 ) ) ;
#4384 = CARTESIAN_POINT ( 'NONE',  ( -108.9451041445662014, 87.93000889276720500, 39.98824025397081527 ) ) ;
#4385 = ORIENTED_EDGE ( 'NONE', *, *, #9464, .F. ) ;
#4386 = CARTESIAN_POINT ( 'NONE',  ( -12.50000000000006750, 1.836970198721034716E-15, 0.000000000000000000 ) ) ;
#4387 = CARTESIAN_POINT ( 'NONE',  ( -63.98537287693023501, 94.20918150411493741, 39.88498244535590231 ) ) ;
#4388 = ORIENTED_EDGE ( 'NONE', *, *, #4505, .T. ) ;
#4389 = EDGE_CURVE ( 'NONE', #11232, #2972, #9240, .T. ) ;
#4390 = ADVANCED_FACE ( 'NONE', ( #16310 ), #4106, .T. ) ;
#4391 = EDGE_LOOP ( 'NONE', ( #8845, #17238, #6617, #15831 ) ) ;
#4392 = EDGE_CURVE ( 'NONE', #16678, #15182, #2294, .T. ) ;
#4393 = CARTESIAN_POINT ( 'NONE',  ( -97.26553299953361886, -115.5756973141631931, 29.67990786120111224 ) ) ;
#4394 = AXIS2_PLACEMENT_3D ( 'NONE', #7878, #3082, #12169 ) ;
#4395 = ORIENTED_EDGE ( 'NONE', *, *, #6979, .F. ) ;
#4396 = CARTESIAN_POINT ( 'NONE',  ( 62.90240729679780429, 1.379293853802413983, 293.5832628385307999 ) ) ;
#4397 = CARTESIAN_POINT ( 'NONE',  ( -32.30548103355237544, 113.3261241031799926, 14.88498244535567672 ) ) ;
#4398 = ORIENTED_EDGE ( 'NONE', *, *, #15882, .T. ) ;
#4399 = CARTESIAN_POINT ( 'NONE',  ( 98.87769906228768946, -132.1136377592460747, 4.931739911029251466 ) ) ;
#4400 = DIRECTION ( 'NONE',  ( 0.000000000000000000, -0.000000000000000000, 1.000000000000000000 ) ) ;
#4401 = EDGE_CURVE ( 'NONE', #2341, #2918, #16758, .T. ) ;
#4402 = EDGE_CURVE ( 'NONE', #10476, #796, #13803, .T. ) ;
#4403 = CARTESIAN_POINT ( 'NONE',  ( -137.9787687278481201, -24.44938394645547675, -11.76118810246814306 ) ) ;
#4404 = DIRECTION ( 'NONE',  ( -0.9511061040868804550, -0.3088643371590125697, 0.000000000000000000 ) ) ;
#4405 = DIRECTION ( 'NONE',  ( 1.000000000000000000, 0.000000000000000000, -0.000000000000000000 ) ) ;
#4406 = DIRECTION ( 'NONE',  ( 1.000000000000000000, 0.000000000000000000, -6.994638739193269649E-15 ) ) ;
#4407 = AXIS2_PLACEMENT_3D ( 'NONE', #16970, #7752, #15539 ) ;
#4408 = FACE_OUTER_BOUND ( 'NONE', #4239, .T. ) ;
#4409 = LINE ( 'NONE', #13710, #9450 ) ;
#4410 = CARTESIAN_POINT ( 'NONE',  ( 97.37676942331995633, -115.5300780475686935, 29.69431357006366312 ) ) ;
#4411 = EDGE_LOOP ( 'NONE', ( #20148, #1362, #14929, #20163 ) ) ;
#4412 = DIRECTION ( 'NONE',  ( 6.982962677686266711E-15, -0.000000000000000000, 1.000000000000000000 ) ) ;
#4413 = DIRECTION ( 'NONE',  ( 1.000000000000000000, 0.000000000000000000, 0.000000000000000000 ) ) ;
#4414 = EDGE_CURVE ( 'NONE', #18388, #11005, #4337, .T. ) ;
#4415 = ORIENTED_EDGE ( 'NONE', *, *, #11994, .F. ) ;
#4416 = VERTEX_POINT ( 'NONE', #9216 ) ;
#4417 = CIRCLE ( 'NONE', #3118, 60.74260934110282051 ) ;
#4418 = ORIENTED_EDGE ( 'NONE', *, *, #11276, .T. ) ;
#4419 = EDGE_CURVE ( 'NONE', #18721, #17815, #6063, .T. ) ;
#4420 = FACE_BOUND ( 'NONE', #11253, .T. ) ;
#4421 = EDGE_LOOP ( 'NONE', ( #11608, #2096, #19039, #5820, #10199 ) ) ;
#4422 = DIRECTION ( 'NONE',  ( 1.000000000000000000, 0.000000000000000000, 0.000000000000000000 ) ) ;
#4423 = DIRECTION ( 'NONE',  ( -6.982962677686266711E-15, 0.000000000000000000, -1.000000000000000000 ) ) ;
#4424 = LINE ( 'NONE', #8822, #1566 ) ;
#4425 = CYLINDRICAL_SURFACE ( 'NONE', #10923, 150.0000000000000284 ) ;
#4426 = DIRECTION ( 'NONE',  ( -0.2225209339563185562, 0.9749279121818227312, 0.000000000000000000 ) ) ;
#4427 = CARTESIAN_POINT ( 'NONE',  ( 60.68567895461851691, -2.629250726500488078, 283.5832628385307999 ) ) ;
#4428 = LINE ( 'NONE', #10658, #10390 ) ;
#4429 = AXIS2_PLACEMENT_3D ( 'NONE', #16843, #19806, #2940 ) ;
#4430 = VERTEX_POINT ( 'NONE', #18537 ) ;
#4431 = DIRECTION ( 'NONE',  ( -0.9749279121818255067, 0.2225209339563057331, 0.000000000000000000 ) ) ;
#4432 = CARTESIAN_POINT ( 'NONE',  ( 0.000000000000000000, 0.000000000000000000, -110.0000000000000000 ) ) ;
#4433 = CARTESIAN_POINT ( 'NONE',  ( 134.4267602304456091, -75.13220794378300127, 5.582054549155156309 ) ) ;
#4434 = CARTESIAN_POINT ( 'NONE',  ( 7.350000000000000533, 5.196152422706627583, 9.000000000000001776 ) ) ;
#4435 = VECTOR ( 'NONE', #18023, 999.9999999999998863 ) ;
#4436 = CARTESIAN_POINT ( 'NONE',  ( -134.7188131032333445, -72.93593548660989256, 30.00000000000000000 ) ) ;
#4437 = CARTESIAN_POINT ( 'NONE',  ( -132.7564094051443249, -84.67399327756427851, 39.12603430846659336 ) ) ;
#4438 = ORIENTED_EDGE ( 'NONE', *, *, #17387, .T. ) ;
#4439 = LINE ( 'NONE', #18674, #6951 ) ;
#4440 = ORIENTED_EDGE ( 'NONE', *, *, #11408, .T. ) ;
#4441 = AXIS2_PLACEMENT_3D ( 'NONE', #17018, #3005, #19972 ) ;
#4442 = ORIENTED_EDGE ( 'NONE', *, *, #8529, .F. ) ;
#4443 = ORIENTED_EDGE ( 'NONE', *, *, #398, .T. ) ;
#4444 = AXIS2_PLACEMENT_3D ( 'NONE', #10484, #15616, #18279 ) ;
#4445 = LINE ( 'NONE', #9043, #13511 ) ;
#4446 = CARTESIAN_POINT ( 'NONE',  ( -110.0000000000000142, 0.000000000000000000, 5.000000000000000888 ) ) ;
#4447 = VERTEX_POINT ( 'NONE', #18648 ) ;
#4448 = CARTESIAN_POINT ( 'NONE',  ( -139.8142396999972163, 1.712230611238718486E-14, -13.33333333333329307 ) ) ;
#4449 = DIRECTION ( 'NONE',  ( 1.000000000000000000, 0.000000000000000000, 0.000000000000000000 ) ) ;
#4450 = EDGE_LOOP ( 'NONE', ( #16483, #11000, #14216, #15566, #17419 ) ) ;
#4451 = CYLINDRICAL_SURFACE ( 'NONE', #3554, 9.000000000000001776 ) ;
#4452 = DIRECTION ( 'NONE',  ( -1.000000000000000000, 0.000000000000000000, 0.000000000000000000 ) ) ;
#4453 = CARTESIAN_POINT ( 'NONE',  ( -23.22641211976288744, -56.12662799072081299, 283.5832628385307999 ) ) ;
#4454 = DIRECTION ( 'NONE',  ( 1.000000000000000000, 0.000000000000000000, 0.000000000000000000 ) ) ;
#4455 = CARTESIAN_POINT ( 'NONE',  ( 140.0000000000000000, 0.000000000000000000, -9.999999999999987566 ) ) ;
#4456 = AXIS2_PLACEMENT_3D ( 'NONE', #4051, #12014, #11910 ) ;
#4457 = VECTOR ( 'NONE', #10856, 1000.000000000000000 ) ;
#4458 = CARTESIAN_POINT ( 'NONE',  ( 128.7737027234268510, -76.92703321535536531, 47.68818876599771528 ) ) ;
#4459 = DIRECTION ( 'NONE',  ( -0.000000000000000000, -0.000000000000000000, 1.000000000000000000 ) ) ;
#4460 = ORIENTED_EDGE ( 'NONE', *, *, #15009, .F. ) ;
#4462 = ORIENTED_EDGE ( 'NONE', *, *, #11357, .F. ) ;
#4461 = CIRCLE ( 'NONE', #3820, 150.0000000000000284 ) ;
#4463 = CARTESIAN_POINT ( 'NONE',  ( -15.91767397667354800, 164.0736214083062805, 60.00000000000000000 ) ) ;
#4464 = VERTEX_POINT ( 'NONE', #15569 ) ;
#4465 = ORIENTED_EDGE ( 'NONE', *, *, #4505, .F. ) ;
#4466 = ADVANCED_FACE ( 'NONE', ( #12281 ), #2788, .F. ) ;
#4467 = DIRECTION ( 'NONE',  ( 0.000000000000000000, 0.000000000000000000, -1.000000000000000000 ) ) ;
#4468 = ORIENTED_EDGE ( 'NONE', *, *, #4969, .F. ) ;
#4469 = CARTESIAN_POINT ( 'NONE',  ( 54.89456854707540856, 30.74413178637212241, 248.9926560891072143 ) ) ;
#4470 = FACE_BOUND ( 'NONE', #2771, .T. ) ;
#4471 = DIRECTION ( 'NONE',  ( -0.9009688679024212554, 0.4338837391175534575, 0.000000000000000000 ) ) ;
#4472 = CYLINDRICAL_SURFACE ( 'NONE', #582, 112.8770930172170210 ) ;
#4473 = VERTEX_POINT ( 'NONE', #4725 ) ;
#4474 = LINE ( 'NONE', #6124, #10002 ) ;
#4475 = LINE ( 'NONE', #2954, #8780 ) ;
#4476 = VERTEX_POINT ( 'NONE', #9008 ) ;
#4477 = AXIS2_PLACEMENT_3D ( 'NONE', #18843, #3290, #9525 ) ;
#4478 = EDGE_CURVE ( 'NONE', #5530, #5045, #11832, .T. ) ;
#4479 = VECTOR ( 'NONE', #17853, 1000.000000000000000 ) ;
#4480 = FACE_OUTER_BOUND ( 'NONE', #17088, .T. ) ;
#4481 = CARTESIAN_POINT ( 'NONE',  ( 0.000000000000000000, 0.000000000000000000, 293.5832628385307999 ) ) ;
#4482 = EDGE_CURVE ( 'NONE', #14025, #4062, #15115, .T. ) ;
#4483 = EDGE_CURVE ( 'NONE', #1866, #1970, #4307, .T. ) ;
#4484 = CARTESIAN_POINT ( 'NONE',  ( -22.29928840491073316, -56.50138340076681231, 293.5832628385307999 ) ) ;
#4485 = CARTESIAN_POINT ( 'NONE',  ( 11.54977938102087620, -57.55901709132175625, 132.4711112102474146 ) ) ;
#4486 = CARTESIAN_POINT ( 'NONE',  ( -133.9068821628478929, -78.54443609883628596, 36.82575673622204704 ) ) ;
#4487 = CARTESIAN_POINT ( 'NONE',  ( 11.54085525628735809, 113.2974248684783163, 39.88498244535537651 ) ) ;
#4488 = EDGE_LOOP ( 'NONE', ( #5982, #886 ) ) ;
#4489 = DIRECTION ( 'NONE',  ( -0.7660444431189813441, 0.6427876096865353661, 0.000000000000000000 ) ) ;
#4490 = CYLINDRICAL_SURFACE ( 'NONE', #5988, 7.500000000000007105 ) ;
#4491 = VERTEX_POINT ( 'NONE', #4622 ) ;
#4492 = VECTOR ( 'NONE', #6022, 1000.000000000000114 ) ;
#4493 = EDGE_LOOP ( 'NONE', ( #8545, #12749, #13580, #10268 ) ) ;
#4494 = EDGE_CURVE ( 'NONE', #15118, #5313, #19856, .T. ) ;
#4495 = CARTESIAN_POINT ( 'NONE',  ( -97.52076053070028649, -133.9271890290945350, 30.74418362133967619 ) ) ;
#4496 = AXIS2_PLACEMENT_3D ( 'NONE', #11200, #14279, #13039 ) ;
#4497 = ORIENTED_EDGE ( 'NONE', *, *, #14769, .F. ) ;
#4498 = CARTESIAN_POINT ( 'NONE',  ( -123.9152654547992825, 71.52026188392119366, -32.55817170788386505 ) ) ;
#4499 = CARTESIAN_POINT ( 'NONE',  ( -39.84224160888947353, -67.36461649554519227, 110.9660488491356887 ) ) ;
#4500 = ORIENTED_EDGE ( 'NONE', *, *, #10003, .F. ) ;
#4501 = CARTESIAN_POINT ( 'NONE',  ( 97.67167802517904818, -133.7293924297389935, 8.145492481267311291 ) ) ;
#4502 = CARTESIAN_POINT ( 'NONE',  ( -68.46530598706769410, 37.93579148621533648, 110.9660488491356887 ) ) ;
#4503 = EDGE_CURVE ( 'NONE', #17764, #8819, #6167, .T. ) ;
#4504 = CIRCLE ( 'NONE', #17269, 60.74260934110282051 ) ;
#4505 = EDGE_CURVE ( 'NONE', #2090, #1965, #20063, .T. ) ;
#4506 = CARTESIAN_POINT ( 'NONE',  ( 11.54085525628735809, 113.2974248684783163, 39.88498244535537651 ) ) ;
#4507 = CIRCLE ( 'NONE', #20180, 62.91752772691707207 ) ;
#4508 = ORIENTED_EDGE ( 'NONE', *, *, #3037, .T. ) ;
#4509 = PLANE ( 'NONE',  #13451 ) ;
#4510 = FACE_OUTER_BOUND ( 'NONE', #5505, .T. ) ;
#4511 = CARTESIAN_POINT ( 'NONE',  ( 0.8038475772933646457, -10.39230484541326582, 2.804506490479260738E-17 ) ) ;
#4512 = CARTESIAN_POINT ( 'NONE',  ( 97.50000000000001421, -115.4778303846449887, 30.00000000000000000 ) ) ;
#4513 = ORIENTED_EDGE ( 'NONE', *, *, #18811, .F. ) ;
#4514 = LINE ( 'NONE', #1134, #7451 ) ;
#4515 = LINE ( 'NONE', #5853, #2073 ) ;
#4516 = VERTEX_POINT ( 'NONE', #12481 ) ;
#4517 = VERTEX_POINT ( 'NONE', #7681 ) ;
#4518 = ADVANCED_FACE ( 'NONE', ( #1135 ), #12385, .F. ) ;
#4519 = APPLICATION_PROTOCOL_DEFINITION ( 'draft international standard', 'automotive_design', 1998, #12986 ) ;
#4520 = AXIS2_PLACEMENT_3D ( 'NONE', #5919, #18089, #4267 ) ;
#4521 = VECTOR ( 'NONE', #4814, 1000.000000000000114 ) ;
#4522 = ORIENTED_EDGE ( 'NONE', *, *, #2782, .F. ) ;
#4523 = CIRCLE ( 'NONE', #17944, 17.50000000000000355 ) ;
#4524 = CARTESIAN_POINT ( 'NONE',  ( -99.98080768883880864, -130.5801677638305023, 3.398603488195621303 ) ) ;
#4525 = CIRCLE ( 'NONE', #6156, 150.0000000000000284 ) ;
#4526 = CARTESIAN_POINT ( 'NONE',  ( -170.2125097089225960, -199.3942630591408260, 40.00000000000000000 ) ) ;
#4527 = ORIENTED_EDGE ( 'NONE', *, *, #7720, .F. ) ;
#4528 = CARTESIAN_POINT ( 'NONE',  ( -107.4999999999999858, -118.5063289449133777, 0.000000000000000000 ) ) ;
#4529 = LINE ( 'NONE', #4636, #137 ) ;
#4530 = CARTESIAN_POINT ( 'NONE',  ( 0.7000608949449920182, 5.693982670708932936, 293.5832628385307999 ) ) ;
#4531 = CARTESIAN_POINT ( 'NONE',  ( -93.96728894855066017, -116.9213660262001611, 48.64206144702517065 ) ) ;
#4532 = EDGE_CURVE ( 'NONE', #1086, #195, #7574, .T. ) ;
#4533 = FACE_OUTER_BOUND ( 'NONE', #18798, .T. ) ;
#4534 = DIRECTION ( 'NONE',  ( 1.000000000000000000, 0.000000000000000000, 0.000000000000000000 ) ) ;
#4535 = EDGE_CURVE ( 'NONE', #1924, #3694, #10846, .T. ) ;
#4536 = CARTESIAN_POINT ( 'NONE',  ( -109.9999999999983515, 285.0000000000000568, 85.00000000000001421 ) ) ;
#4537 = CARTESIAN_POINT ( 'NONE',  ( -134.1862644405548508, -67.03876562297297426, 2.113649378061198458 ) ) ;
#4538 = CARTESIAN_POINT ( 'NONE',  ( 133.2581445365297839, -82.18041427990311831, 1.616105938608680903 ) ) ;
#4539 = CARTESIAN_POINT ( 'NONE',  ( 71.18887634719571622, -147.8252249328912740, 39.99999999999999289 ) ) ;
#4540 = PLANE ( 'NONE',  #3512 ) ;
#4541 = AXIS2_PLACEMENT_3D ( 'NONE', #16045, #17688, #16247 ) ;
#4542 = CARTESIAN_POINT ( 'NONE',  ( -125.5830613944035861, -82.05591916722895007, 41.02171822117688293 ) ) ;
#4543 = AXIS2_PLACEMENT_3D ( 'NONE', #10811, #20229, #9181 ) ;
#4544 = EDGE_CURVE ( 'NONE', #1887, #17975, #4515, .T. ) ;
#4545 = VERTEX_POINT ( 'NONE', #18436 ) ;
#4546 = DIRECTION ( 'NONE',  ( 1.000000000000000000, 0.000000000000000000, 0.000000000000000000 ) ) ;
#4547 = ADVANCED_FACE ( 'NONE', ( #14028 ), #3090, .T. ) ;
#4548 = ORIENTED_EDGE ( 'NONE', *, *, #18828, .F. ) ;
#4549 = ORIENTED_EDGE ( 'NONE', *, *, #34, .F. ) ;
#4550 = AXIS2_PLACEMENT_3D ( 'NONE', #13501, #18032, #10150 ) ;
#4551 = VERTEX_POINT ( 'NONE', #7784 ) ;
#4552 = AXIS2_PLACEMENT_3D ( 'NONE', #1798, #7620, #12318 ) ;
#4553 = CARTESIAN_POINT ( 'NONE',  ( -143.6483359526046968, -15.80165949809716075, 14.64470287550839522 ) ) ;
#4554 = CIRCLE ( 'NONE', #19277, 60.74260934110282051 ) ;
#4555 = CARTESIAN_POINT ( 'NONE',  ( -12.28122767885804301, 61.70726652483831032, 248.9926560891072143 ) ) ;
#4556 = LINE ( 'NONE', #12214, #9738 ) ;
#4557 = ORIENTED_EDGE ( 'NONE', *, *, #4222, .T. ) ;
#4558 = CYLINDRICAL_SURFACE ( 'NONE', #1836, 62.91752772691707207 ) ;
#4559 = CARTESIAN_POINT ( 'NONE',  ( 49.67518383744835120, -60.47951622432767493, 248.9926560891072143 ) ) ;
#4560 = EDGE_LOOP ( 'NONE', ( #19741, #11591, #8740, #15213 ) ) ;
#4561 = CARTESIAN_POINT ( 'NONE',  ( -84.36291539053216582, 110.0674672679312636, -18.84752057685613025 ) ) ;
#4562 = DIRECTION ( 'NONE',  ( 0.9396926207859104263, 0.3420201433256629397, -6.456589605409169071E-15 ) ) ;
#4563 = CARTESIAN_POINT ( 'NONE',  ( 0.000000000000000000, 0.000000000000000000, 0.000000000000000000 ) ) ;
#4564 = CARTESIAN_POINT ( 'NONE',  ( 73.61113626724137760, -92.47916748300480094, 39.88498244535494308 ) ) ;
#4565 = DIRECTION ( 'NONE',  ( -0.5300553768524375320, -0.8479630283625697595, 0.000000000000000000 ) ) ;
#4566 = CARTESIAN_POINT ( 'NONE',  ( 134.1862644405590856, -67.03876562296453301, 37.88635062194084924 ) ) ;
#4567 = DIRECTION ( 'NONE',  ( 0.4693298356057564180, -0.8830229359480272766, 0.000000000000000000 ) ) ;
#4568 = AXIS2_PLACEMENT_3D ( 'NONE', #850, #2597, #17846 ) ;
#4569 = ORIENTED_EDGE ( 'NONE', *, *, #860, .F. ) ;
#4570 = ORIENTED_EDGE ( 'NONE', *, *, #234, .F. ) ;
#4571 = EDGE_LOOP ( 'NONE', ( #12099, #18319, #11264, #15458 ) ) ;
#4572 = EDGE_LOOP ( 'NONE', ( #7337, #19645, #8169, #13432 ) ) ;
#4573 = CARTESIAN_POINT ( 'NONE',  ( -28.63313560863435825, 51.23821591265124198, 110.9660488491356887 ) ) ;
#4574 = PRODUCT_DEFINITION_SHAPE ( 'NONE', 'NONE',  #20247 ) ;
#4575 = ORIENTED_EDGE ( 'NONE', *, *, #6355, .T. ) ;
#4576 = CARTESIAN_POINT ( 'NONE',  ( 68.18670162478805707, 38.41834839689404646, 110.9660488491356887 ) ) ;
#4577 = DIRECTION ( 'NONE',  ( -1.000000000000000000, 0.000000000000000000, 0.000000000000000000 ) ) ;
#4578 = CIRCLE ( 'NONE', #8, 62.91752772691707207 ) ;
#4579 = DIRECTION ( 'NONE',  ( 0.000000000000000000, 0.000000000000000000, 1.000000000000000000 ) ) ;
#4580 =( GEOMETRIC_REPRESENTATION_CONTEXT ( 3 ) GLOBAL_UNCERTAINTY_ASSIGNED_CONTEXT ( ( #7424 ) ) GLOBAL_UNIT_ASSIGNED_CONTEXT ( ( #13400, #2378, #643 ) ) REPRESENTATION_CONTEXT ( 'NONE', 'WORKASPACE' ) );
#4581 = FACE_OUTER_BOUND ( 'NONE', #4010, .T. ) ;
#4582 = EDGE_LOOP ( 'NONE', ( #7260, #4173 ) ) ;
#4583 = AXIS2_PLACEMENT_3D ( 'NONE', #17201, #12472, #12682 ) ;
#4584 = CARTESIAN_POINT ( 'NONE',  ( -4.459628467293889707E-15, 7.573738413550457516, -4.881900264494500874 ) ) ;
#4585 = DIRECTION ( 'NONE',  ( 0.000000000000000000, 0.000000000000000000, 1.000000000000000000 ) ) ;
#4586 = VERTEX_POINT ( 'NONE', #19 ) ;
#4587 = DIRECTION ( 'NONE',  ( 0.2080686897406943681, 0.9781142164131909622, 0.000000000000000000 ) ) ;
#4588 = DIRECTION ( 'NONE',  ( 1.000000000000000000, 0.000000000000000000, 0.000000000000000000 ) ) ;
#4589 = EDGE_CURVE ( 'NONE', #14479, #1, #15446, .T. ) ;
#4590 = CARTESIAN_POINT ( 'NONE',  ( 0.000000000000000000, 7.794228634059940930, -4.500000000000011546 ) ) ;
#4591 = DIRECTION ( 'NONE',  ( 0.8479630283625716469, -0.5300553768524345344, 0.000000000000000000 ) ) ;
#4592 = DIRECTION ( 'NONE',  ( 0.9749279121818227312, 0.2225209339563182231, -0.000000000000000000 ) ) ;
#4593 = LINE ( 'NONE', #18982, #19373 ) ;
#4594 = ORIENTED_EDGE ( 'NONE', *, *, #9383, .T. ) ;
#4595 = DIRECTION ( 'NONE',  ( -1.000000000000000000, 0.000000000000000000, 0.000000000000000000 ) ) ;
#4596 = CARTESIAN_POINT ( 'NONE',  ( -57.94128254008190027, -9.381844291199545438, 132.4711112102474146 ) ) ;
#4597 = ORIENTED_EDGE ( 'NONE', *, *, #15010, .T. ) ;
#4598 = VECTOR ( 'NONE', #7926, 999.9999999999998863 ) ;
#4599 = VERTEX_POINT ( 'NONE', #10642 ) ;
#4600 = DIRECTION ( 'NONE',  ( 0.000000000000000000, 0.000000000000000000, 1.000000000000000000 ) ) ;
#4601 = EDGE_CURVE ( 'NONE', #1034, #5404, #16897, .T. ) ;
#4602 = ORIENTED_EDGE ( 'NONE', *, *, #340, .F. ) ;
#4603 = EDGE_CURVE ( 'NONE', #10224, #5218, #10959, .T. ) ;
#4604 = CARTESIAN_POINT ( 'NONE',  ( -116.4638672662962193, 80.60801470281606385, -34.47751397565569675 ) ) ;
#4605 = DIRECTION ( 'NONE',  ( -1.000000000000000000, -3.320906611023727849E-16, 0.000000000000000000 ) ) ;
#4606 = ORIENTED_EDGE ( 'NONE', *, *, #1907, .T. ) ;
#4607 = CARTESIAN_POINT ( 'NONE',  ( 86.69744916219704578, -122.4084679129025659, -3.219996018902601342 ) ) ;
#4608 = DIRECTION ( 'NONE',  ( -0.9848077530122091305, 0.1736481776669241417, 0.000000000000000000 ) ) ;
#4609 = CIRCLE ( 'NONE', #678, 60.74260934110282051 ) ;
#4610 = AXIS2_PLACEMENT_3D ( 'NONE', #3316, #11075, #19076 ) ;
#4611 = EDGE_CURVE ( 'NONE', #6828, #18284, #8907, .T. ) ;
#4612 = DIRECTION ( 'NONE',  ( 0.7430374143461900838, -0.6692498792541753394, 0.000000000000000000 ) ) ;
#4613 = FACE_BOUND ( 'NONE', #11525, .T. ) ;
#4614 = VERTEX_POINT ( 'NONE', #14340 ) ;
#4615 = LINE ( 'NONE', #9717, #8243 ) ;
#4616 = CARTESIAN_POINT ( 'NONE',  ( 0.000000000000000000, 0.000000000000000000, 283.5832628385307999 ) ) ;
#4617 = LINE ( 'NONE', #10841, #8778 ) ;
#4618 = CARTESIAN_POINT ( 'NONE',  ( 97.83472796452251430, -133.5146506974446652, 32.57231315946213357 ) ) ;
#4619 = EDGE_LOOP ( 'NONE', ( #19256, #12856, #8644, #12571 ) ) ;
#4620 = AXIS2_PLACEMENT_3D ( 'NONE', #17445, #11076, #9846 ) ;
#4621 = LINE ( 'NONE', #14027, #12993 ) ;
#4622 = CARTESIAN_POINT ( 'NONE',  ( -175.8776271403844191, -36.50981547337168109, 60.00000000000000000 ) ) ;
#4623 = ORIENTED_EDGE ( 'NONE', *, *, #6993, .T. ) ;
#4624 = ORIENTED_EDGE ( 'NONE', *, *, #12645, .F. ) ;
#4625 = CARTESIAN_POINT ( 'NONE',  ( 0.000000000000000000, 0.000000000000000000, 0.000000000000000000 ) ) ;
#4626 = EDGE_CURVE ( 'NONE', #18093, #17792, #13468, .T. ) ;
#4627 = EDGE_CURVE ( 'NONE', #13898, #1302, #17521, .T. ) ;
#4628 = AXIS2_PLACEMENT_3D ( 'NONE', #9433, #10852, #4731 ) ;
#4629 = VERTEX_POINT ( 'NONE', #3494 ) ;
#4630 = ADVANCED_FACE ( 'NONE', ( #16080 ), #423, .T. ) ;
#4631 = DIRECTION ( 'NONE',  ( 0.000000000000000000, 0.000000000000000000, 1.000000000000000000 ) ) ;
#4632 = FACE_BOUND ( 'NONE', #11728, .T. ) ;
#4633 = ORIENTED_EDGE ( 'NONE', *, *, #3298, .F. ) ;
#4634 = APPLICATION_CONTEXT ( 'automotive_design' ) ;
#4635 = CARTESIAN_POINT ( 'NONE',  ( 28.94983032429829350, -53.40245231972188833, 293.5832628385307999 ) ) ;
#4636 = CARTESIAN_POINT ( 'NONE',  ( -5.485913980968301296, 1.678175111358176652, 293.5832628385307999 ) ) ;
#4637 = CARTESIAN_POINT ( 'NONE',  ( 124.4460166144179425, -83.75677717049840965, 49.87899788059623063 ) ) ;
#4638 = CARTESIAN_POINT ( 'NONE',  ( -95.64660831657310780, -115.7365562161970587, 34.13915741641437762 ) ) ;
#4639 = DIRECTION ( 'NONE',  ( 0.000000000000000000, 0.000000000000000000, 1.000000000000000000 ) ) ;
#4640 = LINE ( 'NONE', #9713, #7465 ) ;
#4641 = DIRECTION ( 'NONE',  ( 1.000000000000000000, 0.000000000000000000, 0.000000000000000000 ) ) ;
#4642 = CARTESIAN_POINT ( 'NONE',  ( 53.87178215532755132, 28.06680738835045119, 293.5832628385307999 ) ) ;
#4643 = EDGE_CURVE ( 'NONE', #18107, #8936, #16111, .T. ) ;
#4644 = CARTESIAN_POINT ( 'NONE',  ( 123.6072353705854141, -84.98956761793972703, -9.999999999628117919 ) ) ;
#4645 = CARTESIAN_POINT ( 'NONE',  ( 44.79940644582654841, -41.02350267428983699, 293.5832628385307999 ) ) ;
#4646 = DIRECTION ( 'NONE',  ( 0.9009688679024225877, -0.4338837391175509595, 0.000000000000000000 ) ) ;
#4647 = CARTESIAN_POINT ( 'NONE',  ( -129.2715203052800916, -76.16417937454788500, 39.91219297793836063 ) ) ;
#4648 = VERTEX_POINT ( 'NONE', #14637 ) ;
#4649 = CARTESIAN_POINT ( 'NONE',  ( -189.9999999999988916, 285.0000000000000568, 5.000000000000268230 ) ) ;
#4650 = CIRCLE ( 'NONE', #9558, 7.500000000000012434 ) ;
#4651 = ORIENTED_EDGE ( 'NONE', *, *, #19031, .F. ) ;
#4652 = EDGE_CURVE ( 'NONE', #13930, #3067, #6865, .T. ) ;
#4653 = ADVANCED_FACE ( 'NONE', ( #11658 ), #5727, .T. ) ;
#4654 = VERTEX_POINT ( 'NONE', #16381 ) ;
#4655 = ADVANCED_FACE ( 'NONE', ( #622, #2558 ), #2458, .T. ) ;
#4656 = EDGE_CURVE ( 'NONE', #15357, #10563, #9579, .T. ) ;
#4657 = ORIENTED_EDGE ( 'NONE', *, *, #12645, .T. ) ;
#4658 = CARTESIAN_POINT ( 'NONE',  ( -144.8974563261294861, -14.24083055819320087, 7.862900427932681069 ) ) ;
#4659 = CARTESIAN_POINT ( 'NONE',  ( 118.3534152657848608, 114.7431683447366595, 49.99999999999999289 ) ) ;
#4660 = VECTOR ( 'NONE', #14509, 1000.000000000000000 ) ;
#4661 = LINE ( 'NONE', #9662, #11043 ) ;
#4662 = ORIENTED_EDGE ( 'NONE', *, *, #11725, .T. ) ;
#4663 = AXIS2_PLACEMENT_3D ( 'NONE', #16689, #1231, #12170 ) ;
#4664 = CARTESIAN_POINT ( 'NONE',  ( -79.05640494597939494, -127.4758205975444412, 39.99999999999999289 ) ) ;
#4665 = LINE ( 'NONE', #15398, #2599 ) ;
#4666 = ORIENTED_EDGE ( 'NONE', *, *, #6197, .F. ) ;
#4667 = DIRECTION ( 'NONE',  ( 6.982962677686266711E-15, -0.000000000000000000, 1.000000000000000000 ) ) ;
#4668 = B_SPLINE_CURVE_WITH_KNOTS ( 'NONE', 3,
 ( #6236, #12450, #18711, #1313, #4695, #4799, #20029, #3162, #9393, #15639, #1624, #1199, #82, #14094, #12554, #11022, #7442, #17383, #584, #6832, #4906, #14307, #9792, #17781, #17687, #13056, #1928, #9497 ),
 .UNSPECIFIED., .F., .F.,
 ( 4, 2, 2, 2, 2, 2, 2, 2, 2, 2, 2, 2, 2, 4 ),
 ( 2.166383432107200764E-07, 0.004056336319593734953, 0.008112456000844259218, 0.01014051584146950270, 0.01216857568209474792, 0.01622469536334526785, 0.02028081504459578258, 0.02433693472584630077, 0.03244917408834733369, 0.04056141345084836314, 0.04461753313209888827, 0.04867365281334941340, 0.05678589217585046367, 0.06489813153835151394 ),
 .UNSPECIFIED. ) ;
#4669 = DIRECTION ( 'NONE',  ( 1.000000000000000000, 0.000000000000000000, 0.000000000000000000 ) ) ;
#4670 = DIRECTION ( 'NONE',  ( 0.000000000000000000, 0.000000000000000000, -1.000000000000000000 ) ) ;
#4671 = AXIS2_PLACEMENT_3D ( 'NONE', #1750, #7984, #18010 ) ;
#4672 = LINE ( 'NONE', #10894, #4266 ) ;
#4673 = DIRECTION ( 'NONE',  ( -0.8479630283625698706, 0.5300553768524376430, 0.000000000000000000 ) ) ;
#4674 = CARTESIAN_POINT ( 'NONE',  ( 132.5536774537058591, -70.21235394457261236, 42.53698427006028027 ) ) ;
#4675 = DIRECTION ( 'NONE',  ( 1.000000000000000000, 0.000000000000000000, 0.000000000000000000 ) ) ;
#4676 = ORIENTED_EDGE ( 'NONE', *, *, #16658, .T. ) ;
#4677 = ORIENTED_EDGE ( 'NONE', *, *, #17006, .F. ) ;
#4678 = AXIS2_PLACEMENT_3D ( 'NONE', #14852, #19657, #6891 ) ;
#4679 = VECTOR ( 'NONE', #7584, 1000.000000000000000 ) ;
#4680 = VERTEX_POINT ( 'NONE', #11844 ) ;
#4681 = EDGE_CURVE ( 'NONE', #14807, #2821, #719, .T. ) ;
#4682 = VERTEX_POINT ( 'NONE', #14927 ) ;
#4683 = LINE ( 'NONE', #4786, #2079 ) ;
#4684 = ORIENTED_EDGE ( 'NONE', *, *, #17902, .F. ) ;
#4685 = CARTESIAN_POINT ( 'NONE',  ( -54.86954475316242252, 20.84572577951219330, 248.9926560891072143 ) ) ;
#4686 = EDGE_CURVE ( 'NONE', #15800, #3915, #10315, .T. ) ;
#4687 = DIRECTION ( 'NONE',  ( 0.000000000000000000, 0.000000000000000000, 1.000000000000000000 ) ) ;
#4688 = DIRECTION ( 'NONE',  ( 0.000000000000000000, 0.000000000000000000, 1.000000000000000000 ) ) ;
#4689 = CARTESIAN_POINT ( 'NONE',  ( 62.95000000000000284, 6.757601037695096551E-16, -5.035999999999999588 ) ) ;
#4691 = ORIENTED_EDGE ( 'NONE', *, *, #18863, .T. ) ;
#4690 = B_SPLINE_CURVE_WITH_KNOTS ( 'NONE', 3,
 ( #12962, #14205, #590, #9503, #12767, #14510, #16150, #2137, #496, #17287, #9801, #14609, #17490, #189, #6444, #6740, #3465, #18824, #6837, #11231, #19223, #12665, #5210, #11439, #9699, #17694, #9601, #19026, #15948, #8167 ),
 .UNSPECIFIED., .F., .F.,
 ( 4, 2, 2, 2, 2, 2, 2, 2, 2, 2, 2, 2, 2, 2, 4 ),
 ( 0.000000000000000000, 0.002170930610089417522, 0.004341861220178835044, 0.008683722440357699579, 0.01085465305044713488, 0.01302558366053657019, 0.01519651427062600549, 0.01736744488071544079, 0.02170930610089430099, 0.02388023671098372935, 0.02605116732107315772, 0.02822209793116258608, 0.02930756323620730200, 0.03039302854125202139, 0.03473488976143086771 ),
 .UNSPECIFIED. ) ;
#4692 = DIRECTION ( 'NONE',  ( -0.9009688679024161484, -0.4338837391175643932, 0.000000000000000000 ) ) ;
#4693 = CYLINDRICAL_SURFACE ( 'NONE', #10752, 62.91752772691707207 ) ;
#4694 = EDGE_LOOP ( 'NONE', ( #12069, #3860 ) ) ;
#4695 = CARTESIAN_POINT ( 'NONE',  ( -75.78723542615585984, 128.9816322699055888, -15.76009018109207993 ) ) ;
#4696 = CARTESIAN_POINT ( 'NONE',  ( 53.40245231972179596, 28.94983032429848535, 283.5832628385307999 ) ) ;
#4697 = DIRECTION ( 'NONE',  ( -0.000000000000000000, -0.000000000000000000, 1.000000000000000000 ) ) ;
#4698 = CARTESIAN_POINT ( 'NONE',  ( -2.629322876227788264, -60.68773558783006905, 283.5832628385307999 ) ) ;
#4699 = CIRCLE ( 'NONE', #12523, 9.999999999999996447 ) ;
#4700 = DIRECTION ( 'NONE',  ( 0.000000000000000000, 0.000000000000000000, 1.000000000000000000 ) ) ;
#4701 = CARTESIAN_POINT ( 'NONE',  ( -88.41331621464559021, 108.5600746955366844, 32.58608401720460535 ) ) ;
#4702 = VERTEX_POINT ( 'NONE', #13280 ) ;
#4703 = DIRECTION ( 'NONE',  ( -0.000000000000000000, -0.000000000000000000, 1.000000000000000000 ) ) ;
#4704 = AXIS2_PLACEMENT_3D ( 'NONE', #5607, #8376, #995 ) ;
#4705 = ORIENTED_EDGE ( 'NONE', *, *, #18793, .F. ) ;
#4706 = ORIENTED_EDGE ( 'NONE', *, *, #13979, .F. ) ;
#4707 = PLANE ( 'NONE',  #14663 ) ;
#4708 = ORIENTED_EDGE ( 'NONE', *, *, #12218, .T. ) ;
#4709 = CARTESIAN_POINT ( 'NONE',  ( -166.7850001792984926, -190.0000000000000284, 0.000000000000000000 ) ) ;
#4710 = DIRECTION ( 'NONE',  ( 1.000000000000000000, 0.000000000000000000, 0.000000000000000000 ) ) ;
#4711 = ORIENTED_EDGE ( 'NONE', *, *, #8554, .T. ) ;
#4712 = CIRCLE ( 'NONE', #6012, 9.000000000000000000 ) ;
#4713 = CARTESIAN_POINT ( 'NONE',  ( 95.59344839195293275, -116.1516065318577091, 8.743803915443725927 ) ) ;
#4714 = CARTESIAN_POINT ( 'NONE',  ( 0.000000000000000000, 0.000000000000000000, 283.5832628385307999 ) ) ;
#4715 = AXIS2_PLACEMENT_3D ( 'NONE', #1281, #1062, #5788 ) ;
#4716 = FACE_OUTER_BOUND ( 'NONE', #6954, .T. ) ;
#4717 = EDGE_LOOP ( 'NONE', ( #3047, #7884, #5946, #8234 ) ) ;
#4718 = ADVANCED_FACE ( 'NONE', ( #13182 ), #10133, .F. ) ;
#4719 = CARTESIAN_POINT ( 'NONE',  ( -97.49999999999997158, -190.0000000000000000, 40.00000000000000000 ) ) ;
#4720 = DIRECTION ( 'NONE',  ( 0.000000000000000000, 0.000000000000000000, 1.000000000000000000 ) ) ;
#4721 = DIRECTION ( 'NONE',  ( -0.000000000000000000, -1.000000000000000000, -0.000000000000000000 ) ) ;
#4722 = CARTESIAN_POINT ( 'NONE',  ( 82.95463716431549983, -124.9741831325246579, 36.20982395953856070 ) ) ;
#4723 = ORIENTED_EDGE ( 'NONE', *, *, #10609, .T. ) ;
#4724 = PLANE ( 'NONE',  #17598 ) ;
#4725 = CARTESIAN_POINT ( 'NONE',  ( 27.53920554013639688, 73.25972925305640615, 132.4711112102474146 ) ) ;
#4726 = ORIENTED_EDGE ( 'NONE', *, *, #13573, .T. ) ;
#4727 = VECTOR ( 'NONE', #3685, 1000.000000000000000 ) ;
#4728 = B_SPLINE_CURVE_WITH_KNOTS ( 'NONE', 3,
 ( #19799, #5694, #7319, #19697, #12116, #2827, #13657, #4151, #13757, #18271, #10378, #18374, #11911, #15298, #18169, #10190, #6002, #14891, #16641, #16447, #11808, #4351, #2626, #8853 ),
 .UNSPECIFIED., .F., .F.,
 ( 4, 2, 2, 2, 2, 2, 2, 2, 2, 2, 2, 4 ),
 ( 0.000000000000000000, 0.002919511036912186049, 0.005839022073824372099, 0.008758533110736557714, 0.01167804414764874420, 0.01313779966610484351, 0.01459755518456094629, 0.01751706622147310849, 0.01897682173992918872, 0.02043657725838527242, 0.02189633277684135612, 0.02335608829529743635 ),
 .UNSPECIFIED. ) ;
#4729 = ORIENTED_EDGE ( 'NONE', *, *, #7736, .F. ) ;
#4730 = VERTEX_POINT ( 'NONE', #7168 ) ;
#4731 = DIRECTION ( 'NONE',  ( 1.000000000000000000, 0.000000000000000000, 0.000000000000000000 ) ) ;
#4732 = VECTOR ( 'NONE', #1145, 1000.000000000000000 ) ;
#4733 = ORIENTED_EDGE ( 'NONE', *, *, #18231, .T. ) ;
#4734 = EDGE_CURVE ( 'NONE', #8237, #4476, #743, .T. ) ;
#4735 = DIRECTION ( 'NONE',  ( 0.000000000000000000, 0.000000000000000000, 1.000000000000000000 ) ) ;
#4736 = EDGE_CURVE ( 'NONE', #9040, #10253, #3982, .T. ) ;
#4737 = CARTESIAN_POINT ( 'NONE',  ( 56.12853591711344592, -23.22718332831461652, 293.5832628385307999 ) ) ;
#4738 = VERTEX_POINT ( 'NONE', #19541 ) ;
#4739 = AXIS2_PLACEMENT_3D ( 'NONE', #18707, #4692, #10915 ) ;
#4740 = DIRECTION ( 'NONE',  ( -0.7881095627315599650, -0.6155349844899714595, 0.000000000000000000 ) ) ;
#4741 = LINE ( 'NONE', #18859, #3725 ) ;
#4742 = CARTESIAN_POINT ( 'NONE',  ( 134.9931224044436817, -65.39776452395021522, 32.90319768524037158 ) ) ;
#4743 = CARTESIAN_POINT ( 'NONE',  ( -98.87769906228751893, -132.1136377592408735, 35.06826008897053271 ) ) ;
#4744 = AXIS2_PLACEMENT_3D ( 'NONE', #9033, #4129, #16145 ) ;
#4745 = LINE ( 'NONE', #15693, #8691 ) ;
#4746 = CARTESIAN_POINT ( 'NONE',  ( -139.6619321461413961, 9.919133126256308941, 23.58131293488760249 ) ) ;
#4747 = ADVANCED_FACE ( 'NONE', ( #13383 ), #14831, .F. ) ;
#4748 = CARTESIAN_POINT ( 'NONE',  ( -38.35506425062487779, -44.43084819159262366, 110.7293897666001214 ) ) ;
#4749 = ADVANCED_FACE ( 'NONE', ( #19636 ), #1011, .F. ) ;
#4750 = DIRECTION ( 'NONE',  ( 1.000000000000000000, 0.000000000000000000, 0.000000000000000000 ) ) ;
#4751 = CYLINDRICAL_SURFACE ( 'NONE', #3194, 112.8770930172170210 ) ;
#4752 = CARTESIAN_POINT ( 'NONE',  ( -130.0495322079418372, -74.74954793754226046, 46.42469753870267368 ) ) ;
#4753 = VERTEX_POINT ( 'NONE', #17817 ) ;
#4754 = EDGE_CURVE ( 'NONE', #20158, #17735, #8594, .T. ) ;
#4755 = PRODUCT_DEFINITION_SHAPE ( 'NONE', 'NONE',  #8640 ) ;
#4756 = DIRECTION ( 'NONE',  ( 0.3420201433256726542, -0.9396926207859069846, 0.000000000000000000 ) ) ;
#4757 = AXIS2_PLACEMENT_3D ( 'NONE', #17706, #15961, #5126 ) ;
#4758 = ORIENTED_EDGE ( 'NONE', *, *, #12594, .F. ) ;
#4759 = ORIENTED_EDGE ( 'NONE', *, *, #548, .T. ) ;
#4760 = EDGE_CURVE ( 'NONE', #19487, #18358, #3710, .T. ) ;
#4761 = VERTEX_POINT ( 'NONE', #18013 ) ;
#4762 = CARTESIAN_POINT ( 'NONE',  ( -143.5145034128292707, -15.97856208114589016, 15.09934064724655833 ) ) ;
#4763 = VECTOR ( 'NONE', #16441, 1000.000000000000000 ) ;
#4764 = DIRECTION ( 'NONE',  ( 0.4999999999999888978, 0.8660254037844449249, 0.000000000000000000 ) ) ;
#4765 = CARTESIAN_POINT ( 'NONE',  ( 12.78021302872850562, -77.21438937758507848, 248.9926560891072143 ) ) ;
#4767 = CARTESIAN_POINT ( 'NONE',  ( 27.90514497005392869, -110.4119590718113244, 39.88498244535525572 ) ) ;
#4766 = VECTOR ( 'NONE', #14523, 1000.000000000000000 ) ;
#4768 = FACE_OUTER_BOUND ( 'NONE', #13643, .T. ) ;
#4769 = DIRECTION ( 'NONE',  ( -0.7881095627315599650, -0.6155349844899714595, 0.000000000000000000 ) ) ;
#4770 = CARTESIAN_POINT ( 'NONE',  ( 11.54085525628718401, 113.2974248684783163, 14.88498244535537296 ) ) ;
#4771 = DIRECTION ( 'NONE',  ( 0.000000000000000000, 0.000000000000000000, 1.000000000000000000 ) ) ;
#4772 = EDGE_CURVE ( 'NONE', #13894, #15168, #6962, .T. ) ;
#4773 = DIRECTION ( 'NONE',  ( -0.000000000000000000, -0.000000000000000000, 1.000000000000000000 ) ) ;
#4774 = DIRECTION ( 'NONE',  ( -6.982962677686266711E-15, 0.000000000000000000, -1.000000000000000000 ) ) ;
#4775 = EDGE_CURVE ( 'NONE', #9982, #8985, #9914, .T. ) ;
#4776 = ADVANCED_FACE ( 'NONE', ( #2762 ), #4490, .F. ) ;
#4777 = ORIENTED_EDGE ( 'NONE', *, *, #4870, .F. ) ;
#4778 = CARTESIAN_POINT ( 'NONE',  ( 134.5315346870376629, -74.37329574991311176, 33.61297800067708152 ) ) ;
#4779 = CARTESIAN_POINT ( 'NONE',  ( 57.61823435390807902, 19.23677882349220880, 283.5832628385307999 ) ) ;
#4780 = VECTOR ( 'NONE', #756, 1000.000000000000000 ) ;
#4781 = ORIENTED_EDGE ( 'NONE', *, *, #2859, .F. ) ;
#4782 = ORIENTED_EDGE ( 'NONE', *, *, #8914, .F. ) ;
#4783 = ORIENTED_EDGE ( 'NONE', *, *, #10156, .F. ) ;
#4784 = ORIENTED_EDGE ( 'NONE', *, *, #9415, .T. ) ;
#4785 = AXIS2_PLACEMENT_3D ( 'NONE', #1841, #13909, #2974 ) ;
#4786 = CARTESIAN_POINT ( 'NONE',  ( 1.379293853801755176, -62.90240729679781850, 293.5832628385307999 ) ) ;
#4787 = EDGE_CURVE ( 'NONE', #16297, #9534, #10616, .T. ) ;
#4788 = VERTEX_POINT ( 'NONE', #15437 ) ;
#4789 = DIRECTION ( 'NONE',  ( 0.000000000000000000, 0.000000000000000000, -1.000000000000000000 ) ) ;
#4790 = CARTESIAN_POINT ( 'NONE',  ( -98.70372244599820988, -132.3513910121202741, 34.77299687110840409 ) ) ;
#4791 = CARTESIAN_POINT ( 'NONE',  ( 7.350000000000001421, 0.000000000000000000, 0.000000000000000000 ) ) ;
#4792 = DIRECTION ( 'NONE',  ( -0.9511061040868794558, -0.3088643371590157338, 0.000000000000000000 ) ) ;
#4793 = EDGE_LOOP ( 'NONE', ( #840, #13871, #13576, #16723 ) ) ;
#4794 = CARTESIAN_POINT ( 'NONE',  ( -166.7850001792984926, -190.0000000000000284, 40.00000000000000000 ) ) ;
#4795 = DIRECTION ( 'NONE',  ( 0.000000000000000000, 0.000000000000000000, 1.000000000000000000 ) ) ;
#4796 = VECTOR ( 'NONE', #18764, 1000.000000000000000 ) ;
#4797 = ORIENTED_EDGE ( 'NONE', *, *, #19975, .F. ) ;
#4798 = VECTOR ( 'NONE', #2487, 1000.000000000000000 ) ;
#4799 = CARTESIAN_POINT ( 'NONE',  ( -76.78599263319790680, 128.0787319494822896, -17.29805744153746616 ) ) ;
#4800 = DIRECTION ( 'NONE',  ( -0.3427509529624096496, -0.9394263059140723904, 0.000000000000000000 ) ) ;
#4801 = ADVANCED_FACE ( 'NONE', ( #2964 ), #13690, .T. ) ;
#4802 = EDGE_CURVE ( 'NONE', #17872, #9691, #13795, .T. ) ;
#4803 = DIRECTION ( 'NONE',  ( -0.6427876096865353661, -0.7660444431189813441, 0.000000000000000000 ) ) ;
#4804 = AXIS2_PLACEMENT_3D ( 'NONE', #391, #6643, #12868 ) ;
#4805 = FACE_OUTER_BOUND ( 'NONE', #1687, .T. ) ;
#4806 = DIRECTION ( 'NONE',  ( 0.000000000000000000, 0.000000000000000000, -1.000000000000000000 ) ) ;
#4807 = DIRECTION ( 'NONE',  ( -0.000000000000000000, -0.000000000000000000, 1.000000000000000000 ) ) ;
#4808 = EDGE_CURVE ( 'NONE', #3935, #5836, #7657, .T. ) ;
#4809 = ORIENTED_EDGE ( 'NONE', *, *, #16004, .T. ) ;
#4810 = CARTESIAN_POINT ( 'NONE',  ( 0.000000000000000000, 0.000000000000000000, 83.57543755549745867 ) ) ;
#4811 = EDGE_LOOP ( 'NONE', ( #16003, #8956, #15930, #10927 ) ) ;
#4812 = VECTOR ( 'NONE', #10305, 1000.000000000000000 ) ;
#4813 = VERTEX_POINT ( 'NONE', #18510 ) ;
#4814 = DIRECTION ( 'NONE',  ( -0.000000000000000000, 0.5000000000000012212, 0.8660254037844379305 ) ) ;
#4815 = AXIS2_PLACEMENT_3D ( 'NONE', #11950, #3987, #3796 ) ;
#4816 = EDGE_LOOP ( 'NONE', ( #13429, #1663, #8595, #12133 ) ) ;
#4817 = CARTESIAN_POINT ( 'NONE',  ( 0.000000000000000000, 0.000000000000000000, -115.0000000000000000 ) ) ;
#4818 = DIRECTION ( 'NONE',  ( 0.000000000000000000, 0.000000000000000000, 1.000000000000000000 ) ) ;
#4819 = AXIS2_PLACEMENT_3D ( 'NONE', #10172, #16521, #14872 ) ;
#4820 = VERTEX_POINT ( 'NONE', #7453 ) ;
#4821 = CARTESIAN_POINT ( 'NONE',  ( 97.34896704141638679, -115.5410409672066692, 10.27529861476682527 ) ) ;
#4822 = CARTESIAN_POINT ( 'NONE',  ( 65.74260934110282051, 8.909359647227704685E-15, 293.5832628385307999 ) ) ;
#4823 = CARTESIAN_POINT ( 'NONE',  ( -23.19741967113669290, 4.658826548058537576, 14.88498244535561277 ) ) ;
#4824 = DIRECTION ( 'NONE',  ( -0.9396926207859068736, -0.3420201433256725987, 0.000000000000000000 ) ) ;
#4825 = VERTEX_POINT ( 'NONE', #17346 ) ;
#4826 = DIRECTION ( 'NONE',  ( -0.9271237148521547233, 0.3747554100459928872, 0.000000000000000000 ) ) ;
#4827 = DIRECTION ( 'NONE',  ( -0.000000000000000000, -0.000000000000000000, -1.000000000000000000 ) ) ;
#4828 = CARTESIAN_POINT ( 'NONE',  ( 0.8220851292435327196, 62.91215678473957240, 132.4711112102474146 ) ) ;
#4829 = CARTESIAN_POINT ( 'NONE',  ( 97.50000000000001421, -133.9542832455803989, 30.75506667725924714 ) ) ;
#4830 = CIRCLE ( 'NONE', #9721, 60.74260934110282051 ) ;
#4831 = EDGE_LOOP ( 'NONE', ( #17378, #6527, #10797, #20027 ) ) ;
#4832 =( BOUNDED_CURVE ( )  B_SPLINE_CURVE ( 3, ( #6109, #1179, #12120, #15513 ),
 .UNSPECIFIED., .F., .F. ) 
 B_SPLINE_CURVE_WITH_KNOTS ( ( 4, 4 ),
 ( 1.920639998745670596, 3.141592653589794004 ),
 .UNSPECIFIED. ) 
 CURVE ( )  GEOMETRIC_REPRESENTATION_ITEM ( )  RATIONAL_B_SPLINE_CURVE ( ( 1.000000000000000000, 0.8795833682608492632, 0.8795833682608492632, 1.000000000000000000 ) ) 
 REPRESENTATION_ITEM ( '' )  );
#4833 = AXIS2_PLACEMENT_3D ( 'NONE', #1933, #13351, #2332 ) ;
#4834 = CARTESIAN_POINT ( 'NONE',  ( 36.99514631729018532, -48.17959877923561862, 283.5832628385307999 ) ) ;
#4835 = CARTESIAN_POINT ( 'NONE',  ( -82.03494826539123608, 125.5818021290787669, 33.61186608239164997 ) ) ;
#4836 = VECTOR ( 'NONE', #4979, 1000.000000000000000 ) ;
#4837 = ORIENTED_EDGE ( 'NONE', *, *, #5365, .F. ) ;
#4838 = VERTEX_POINT ( 'NONE', #10724 ) ;
#4839 = ORIENTED_EDGE ( 'NONE', *, *, #13152, .F. ) ;
#4840 = CARTESIAN_POINT ( 'NONE',  ( 0.000000000000000000, 0.000000000000000000, 0.000000000000000000 ) ) ;
#4841 = VERTEX_POINT ( 'NONE', #9089 ) ;
#4842 = DIRECTION ( 'NONE',  ( -6.982962677686266711E-15, 0.000000000000000000, -1.000000000000000000 ) ) ;
#4843 = FACE_OUTER_BOUND ( 'NONE', #1555, .T. ) ;
#4844 = ORIENTED_EDGE ( 'NONE', *, *, #2578, .T. ) ;
#4845 = CARTESIAN_POINT ( 'NONE',  ( 5.729042578294381016, 0.2993243175132339062, 293.5832628385307999 ) ) ;
#4846 = CARTESIAN_POINT ( 'NONE',  ( -107.4999999999999716, -200.0000000000000000, 0.000000000000000000 ) ) ;
#4847 = CARTESIAN_POINT ( 'NONE',  ( -97.49999999999997158, -133.9542832461881972, 9.999999999999996447 ) ) ;
#4848 = AXIS2_PLACEMENT_3D ( 'NONE', #9762, #3222, #9466 ) ;
#4849 = VECTOR ( 'NONE', #13446, 1000.000000000000114 ) ;
#4850 = CARTESIAN_POINT ( 'NONE',  ( -95.44734317237906396, -116.0775604631401450, 32.45031486599465609 ) ) ;
#4851 = DIRECTION ( 'NONE',  ( 0.1736481776669404620, -0.9848077530122062440, 0.000000000000000000 ) ) ;
#4852 = CARTESIAN_POINT ( 'NONE',  ( -139.7878999548352965, 7.953874699751952271, 23.37681481726362875 ) ) ;
#4853 = CYLINDRICAL_SURFACE ( 'NONE', #8676, 3.224098631618460331 ) ;
#4854 = CARTESIAN_POINT ( 'NONE',  ( -149.9962010962228476, 1.232532946391591056, 4.363522735748509795 ) ) ;
#4855 = CARTESIAN_POINT ( 'NONE',  ( 0.000000000000000000, 164.0736214083062805, 60.00000000000000000 ) ) ;
#4856 = DIRECTION ( 'NONE',  ( 6.982962677686266711E-15, -0.000000000000000000, 1.000000000000000000 ) ) ;
#4857 = CARTESIAN_POINT ( 'NONE',  ( -123.6072353705779250, -84.98956761795039938, 49.99999999963072383 ) ) ;
#4858 = ADVANCED_FACE ( 'NONE', ( #16976 ), #2661, .F. ) ;
#4859 = VERTEX_POINT ( 'NONE', #17078 ) ;
#4860 = B_SPLINE_CURVE_WITH_KNOTS ( 'NONE', 3,
 ( #4978, #6410, #17463, #11096, #17359, #15817, #5278, #3434, #17758, #2107, #3333, #6811, #13038, #19294, #18996, #9671, #9771, #11505, #3731, #16022, #2006, #9972, #160, #15918, #14381, #12631 ),
 .UNSPECIFIED., .F., .F.,
 ( 4, 2, 2, 2, 2, 2, 2, 2, 2, 2, 2, 2, 4 ),
 ( 0.000000000000000000, 0.001429785831555268043, 0.002144678747332922665, 0.002859571663110577287, 0.004289357494665905178, 0.005719143326221231768, 0.007148929157776559226, 0.008578714989331886684, 0.01143828665244248435, 0.01429785831555308029, 0.01572764414710837999, 0.01715742997866371439, 0.02287657330488496871 ),
 .UNSPECIFIED. ) ;
#4861 = CARTESIAN_POINT ( 'NONE',  ( -159.9599531637108782, -36.50981547337168109, 39.99999999999999289 ) ) ;
#4862 = VECTOR ( 'NONE', #18366, 1000.000000000000000 ) ;
#4863 = CIRCLE ( 'NONE', #7450, 99.99999999999997158 ) ;
#4864 = VECTOR ( 'NONE', #12584, 1000.000000000000000 ) ;
#4865 = ORIENTED_EDGE ( 'NONE', *, *, #14259, .T. ) ;
#4866 = ORIENTED_EDGE ( 'NONE', *, *, #3956, .T. ) ;
#4867 = ADVANCED_FACE ( 'NONE', ( #20040, #7757 ), #6245, .F. ) ;
#4868 = ORIENTED_EDGE ( 'NONE', *, *, #14413, .T. ) ;
#4869 = EDGE_CURVE ( 'NONE', #9831, #18211, #9254, .T. ) ;
#4870 = EDGE_CURVE ( 'NONE', #5317, #13849, #11547, .T. ) ;
#4871 = LINE ( 'NONE', #15708, #18774 ) ;
#4872 = CARTESIAN_POINT ( 'NONE',  ( 0.000000000000000000, 164.0736214083062805, 39.99999999999999289 ) ) ;
#4873 = VECTOR ( 'NONE', #11877, 1000.000000000000000 ) ;
#4874 = CARTESIAN_POINT ( 'NONE',  ( -150.0000000000000000, 0.000000000000000000, 5.000000000000011546 ) ) ;
#4875 = TOROIDAL_SURFACE ( 'NONE', #9753, 110.0000000000000142, 30.00000000000000000 ) ;
#4876 = TOROIDAL_SURFACE ( 'NONE', #14348, 110.0000000000000142, 40.00000000000000000 ) ;
#4877 = DIRECTION ( 'NONE',  ( -1.000000000000000000, 0.000000000000000000, 0.000000000000000000 ) ) ;
#4878 = AXIS2_PLACEMENT_3D ( 'NONE', #16541, #19695, #19597 ) ;
#4879 = CARTESIAN_POINT ( 'NONE',  ( 0.000000000000000000, 0.000000000000000000, 283.5832628385307999 ) ) ;
#4880 = CARTESIAN_POINT ( 'NONE',  ( 27.53920554013639688, 73.25972925305639194, 111.4180192758974499 ) ) ;
#4881 = CARTESIAN_POINT ( 'NONE',  ( 74.01264520835154315, -25.47058595421579952, 132.4711112102474146 ) ) ;
#4882 = DIRECTION ( 'NONE',  ( -0.000000000000000000, -0.000000000000000000, 1.000000000000000000 ) ) ;
#4883 = EDGE_CURVE ( 'NONE', #15236, #2173, #16674, .T. ) ;
#4884 = ORIENTED_EDGE ( 'NONE', *, *, #6362, .F. ) ;
#4885 = CARTESIAN_POINT ( 'NONE',  ( 134.9140359355661758, -65.56103033673134917, 33.73225304246028600 ) ) ;
#4886 = DIRECTION ( 'NONE',  ( -6.982962677686266711E-15, 0.000000000000000000, -1.000000000000000000 ) ) ;
#4887 = ORIENTED_EDGE ( 'NONE', *, *, #17334, .F. ) ;
#4888 = ORIENTED_EDGE ( 'NONE', *, *, #19843, .T. ) ;
#4889 = ORIENTED_EDGE ( 'NONE', *, *, #2361, .F. ) ;
#4890 = AXIS2_PLACEMENT_3D ( 'NONE', #488, #8255, #8355 ) ;
#4891 = VECTOR ( 'NONE', #12654, 1000.000000000000227 ) ;
#4892 = ORIENTED_EDGE ( 'NONE', *, *, #1393, .F. ) ;
#4893 = CARTESIAN_POINT ( 'NONE',  ( -68.18670162478832708, -38.41834839689356329, 248.9926560891072143 ) ) ;
#4894 = EDGE_CURVE ( 'NONE', #8253, #7528, #6336, .T. ) ;
#4895 = ORIENTED_EDGE ( 'NONE', *, *, #11106, .T. ) ;
#4896 = DIRECTION ( 'NONE',  ( -0.5000000000000069944, 0.8660254037844344888, -0.000000000000000000 ) ) ;
#4897 = ADVANCED_FACE ( 'NONE', ( #13582 ), #19830, .T. ) ;
#4898 = EDGE_CURVE ( 'NONE', #9304, #18854, #6038, .T. ) ;
#4899 = CARTESIAN_POINT ( 'NONE',  ( -102.6638558517306166, -126.6149147318370041, 38.77018177895282491 ) ) ;
#4900 = CARTESIAN_POINT ( 'NONE',  ( 7.500000000000006217, 164.0736214083062805, 39.99999999999999289 ) ) ;
#4901 = DIRECTION ( 'NONE',  ( 1.000000000000000000, 0.000000000000000000, 0.000000000000000000 ) ) ;
#4902 = ORIENTED_EDGE ( 'NONE', *, *, #12245, .F. ) ;
#4903 = CARTESIAN_POINT ( 'NONE',  ( 133.3341203894445641, -68.71829099011287667, -0.6771230101111865851 ) ) ;
#4904 = CARTESIAN_POINT ( 'NONE',  ( -76.92888220842476699, 14.39940464655786201, 112.0427633081292385 ) ) ;
#4905 = ORIENTED_EDGE ( 'NONE', *, *, #12490, .F. ) ;
#4906 = CARTESIAN_POINT ( 'NONE',  ( -96.67593751107419564, 105.2677311041483392, -32.72576864185690226 ) ) ;
#4907 = DIRECTION ( 'NONE',  ( -0.8830229359480271656, -0.4693298356057563625, 0.000000000000000000 ) ) ;
#4908 = CIRCLE ( 'NONE', #11420, 17.50000000000000355 ) ;
#4909 = AXIS2_PLACEMENT_3D ( 'NONE', #11090, #12626, #15604 ) ;
#4910 = CARTESIAN_POINT ( 'NONE',  ( -67.36461649554505016, 39.84224160888970800, 110.9660488491356887 ) ) ;
#4911 = EDGE_CURVE ( 'NONE', #8175, #6529, #5939, .T. ) ;
#4912 = CARTESIAN_POINT ( 'NONE',  ( 159.9599531637113330, -36.50981547336952104, 60.00000000000000000 ) ) ;
#4913 = CARTESIAN_POINT ( 'NONE',  ( -75.02042969003670692, 118.2029424473213197, 2.920782463702978671 ) ) ;
#4914 = ORIENTED_EDGE ( 'NONE', *, *, #17890, .F. ) ;
#4915 = DIRECTION ( 'NONE',  ( 0.000000000000000000, 0.000000000000000000, -1.000000000000000000 ) ) ;
#4916 = EDGE_LOOP ( 'NONE', ( #13738, #7816, #6521, #9856 ) ) ;
#4917 = ORIENTED_EDGE ( 'NONE', *, *, #2729, .T. ) ;
#4918 = DIRECTION ( 'NONE',  ( 0.6427876096865353661, 0.7660444431189813441, -0.000000000000000000 ) ) ;
#4919 = ADVANCED_FACE ( 'NONE', ( #7555 ), #12770, .F. ) ;
#4920 = ORIENTED_EDGE ( 'NONE', *, *, #8721, .F. ) ;
#4921 = EDGE_CURVE ( 'NONE', #2071, #5114, #15746, .T. ) ;
#4922 = AXIS2_PLACEMENT_3D ( 'NONE', #18947, #11045, #8183 ) ;
#4923 = ADVANCED_FACE ( 'NONE', ( #11132 ), #9401, .F. ) ;
#4924 = ADVANCED_FACE ( 'NONE', ( #16056 ), #9701, .F. ) ;
#4925 = CARTESIAN_POINT ( 'NONE',  ( -135.9903138276601737, 55.59603877235524294, -25.41015113300352368 ) ) ;
#4926 = CARTESIAN_POINT ( 'NONE',  ( 0.000000000000000000, 0.000000000000000000, 49.99999999999999289 ) ) ;
#4927 = EDGE_LOOP ( 'NONE', ( #19709, #10613, #2737, #12940 ) ) ;
#4928 = CARTESIAN_POINT ( 'NONE',  ( 70.38703763562291726, -92.47916748300480094, 39.88498244535495729 ) ) ;
#4929 = DIRECTION ( 'NONE',  ( 0.000000000000000000, 0.000000000000000000, 1.000000000000000000 ) ) ;
#4930 = CARTESIAN_POINT ( 'NONE',  ( -38.41834839689332171, 68.18670162478844077, 248.9926560891072143 ) ) ;
#4931 = CARTESIAN_POINT ( 'NONE',  ( 44.43084819159276577, -38.35506425062471436, 132.4711112102474146 ) ) ;
#4932 = VECTOR ( 'NONE', #15742, 1000.000000000000114 ) ;
#4933 = CARTESIAN_POINT ( 'NONE',  ( 0.000000000000000000, 0.000000000000000000, 293.5832628385307999 ) ) ;
#4934 = ORIENTED_EDGE ( 'NONE', *, *, #10382, .F. ) ;
#4935 = LINE ( 'NONE', #6568, #18715 ) ;
#4936 = DIRECTION ( 'NONE',  ( 0.3088643371590157338, -0.9511061040868794558, 0.000000000000000000 ) ) ;
#4937 = CARTESIAN_POINT ( 'NONE',  ( -110.0000000000000142, 275.0000000000000000, -82.50000000000001421 ) ) ;
#4938 = CIRCLE ( 'NONE', #9509, 7.500000000000007105 ) ;
#4939 = CARTESIAN_POINT ( 'NONE',  ( 99.73778183779745632, -112.0462389701484511, 50.00000000040667203 ) ) ;
#4940 = EDGE_LOOP ( 'NONE', ( #18354, #4934, #19786, #15681 ) ) ;
#4941 = DIRECTION ( 'NONE',  ( 1.000000000000000000, 0.000000000000000000, -6.977185866873308817E-15 ) ) ;
#4942 = CARTESIAN_POINT ( 'NONE',  ( -70.84156478054282502, 132.2175582643460245, 13.17469413506393217 ) ) ;
#4943 = ORIENTED_EDGE ( 'NONE', *, *, #10223, .T. ) ;
#4944 = ORIENTED_EDGE ( 'NONE', *, *, #14517, .F. ) ;
#4945 = ORIENTED_EDGE ( 'NONE', *, *, #3519, .T. ) ;
#4946 = APPLICATION_PROTOCOL_DEFINITION ( 'draft international standard', 'automotive_design', 1998, #9854 ) ;
#4947 = EDGE_LOOP ( 'NONE', ( #12489, #19723, #14734, #18986 ) ) ;
#4948 = DIRECTION ( 'NONE',  ( -1.000000000000000000, 0.000000000000000000, 0.000000000000000000 ) ) ;
#4949 = DIRECTION ( 'NONE',  ( 0.000000000000000000, 0.000000000000000000, 1.000000000000000000 ) ) ;
#4950 = EDGE_LOOP ( 'NONE', ( #3759, #1197, #17031, #7888 ) ) ;
#4951 = AXIS2_PLACEMENT_3D ( 'NONE', #4539, #6081, #10871 ) ;
#4952 = DIRECTION ( 'NONE',  ( 6.982962677686266711E-15, -0.000000000000000000, 1.000000000000000000 ) ) ;
#4953 = CARTESIAN_POINT ( 'NONE',  ( -17.50000000000001066, 2.143131898507869431E-15, 4.999999999999948486 ) ) ;
#4954 = DIRECTION ( 'NONE',  ( 0.8660254037844328234, 0.5000000000000101030, 0.000000000000000000 ) ) ;
#4955 = ADVANCED_FACE ( 'NONE', ( #10928 ), #18826, .F. ) ;
#4956 = CARTESIAN_POINT ( 'NONE',  ( -102.7594822686546507, -126.4624059756590810, 38.81042005228335512 ) ) ;
#4957 = DIRECTION ( 'NONE',  ( -0.7818314824680221431, -0.6234898018587431423, 0.000000000000000000 ) ) ;
#4958 = CARTESIAN_POINT ( 'NONE',  ( -30.05702882063063086, -50.41613078340792242, 110.9660488491356887 ) ) ;
#4959 = CARTESIAN_POINT ( 'NONE',  ( -189.9999999999988916, 275.0000000000000000, 5.000000000000268230 ) ) ;
#4960 = DIRECTION ( 'NONE',  ( 1.000000000000000000, 0.000000000000000000, 0.000000000000000000 ) ) ;
#4961 = CARTESIAN_POINT ( 'NONE',  ( -6.191009641800249597, -26.42934155884823255, 39.88498244535549730 ) ) ;
#4962 = DIRECTION ( 'NONE',  ( -1.000000000000000000, 0.000000000000000000, 0.000000000000000000 ) ) ;
#4963 = ORIENTED_EDGE ( 'NONE', *, *, #10236, .F. ) ;
#4964 = AXIS2_PLACEMENT_3D ( 'NONE', #6977, #16300, #13196 ) ;
#4965 = CARTESIAN_POINT ( 'NONE',  ( -125.0787927518813518, 50.79647550709884030, -26.58908968555560648 ) ) ;
#4966 = VECTOR ( 'NONE', #13839, 1000.000000000000000 ) ;
#4967 = ORIENTED_EDGE ( 'NONE', *, *, #19795, .F. ) ;
#4968 = ORIENTED_EDGE ( 'NONE', *, *, #11278, .F. ) ;
#4969 = EDGE_CURVE ( 'NONE', #8266, #9691, #12668, .T. ) ;
#4970 = CARTESIAN_POINT ( 'NONE',  ( 0.07661102881317106983, -6.914460432017385472, -6.023803224821242530 ) ) ;
#4971 = DIRECTION ( 'NONE',  ( 0.000000000000000000, 0.000000000000000000, 1.000000000000000000 ) ) ;
#4972 = LINE ( 'NONE', #7919, #196 ) ;
#4973 = CARTESIAN_POINT ( 'NONE',  ( 4.811834253409037032, 3.123743752084113812, 293.5832628385307999 ) ) ;
#4974 = ORIENTED_EDGE ( 'NONE', *, *, #11538, .T. ) ;
#4975 = DIRECTION ( 'NONE',  ( 1.000000000000000000, 0.000000000000000000, 0.000000000000000000 ) ) ;
#4976 = DIRECTION ( 'NONE',  ( -0.000000000000000000, -0.000000000000000000, 1.000000000000000000 ) ) ;
#4977 = DIRECTION ( 'NONE',  ( -1.000000000000000000, 0.000000000000000000, 0.000000000000000000 ) ) ;
#4978 = CARTESIAN_POINT ( 'NONE',  ( 97.50000000000001421, -133.9542832461881119, 30.00000000000000000 ) ) ;
#4979 = DIRECTION ( 'NONE',  ( 0.8660254037844328234, 0.5000000000000101030, 0.000000000000000000 ) ) ;
#4980 = ORIENTED_EDGE ( 'NONE', *, *, #9415, .F. ) ;
#4981 = ADVANCED_FACE ( 'NONE', ( #17188 ), #5113, .F. ) ;
#4982 = CARTESIAN_POINT ( 'NONE',  ( 134.7188131032333729, -72.93593548660993520, 30.00000000000000000 ) ) ;
#4983 = CARTESIAN_POINT ( 'NONE',  ( -110.0000000000000142, 275.0000000000000000, -94.99999999999997158 ) ) ;
#4984 = ORIENTED_EDGE ( 'NONE', *, *, #14641, .T. ) ;
#4985 = ORIENTED_EDGE ( 'NONE', *, *, #5809, .F. ) ;
#4986 = ORIENTED_EDGE ( 'NONE', *, *, #6188, .T. ) ;
#4987 = EDGE_LOOP ( 'NONE', ( #7887, #4844, #12073, #17622 ) ) ;
#4988 = DIRECTION ( 'NONE',  ( -0.8660254037844380415, -0.5000000000000009992, 0.000000000000000000 ) ) ;
#4989 = VECTOR ( 'NONE', #17838, 999.9999999999998863 ) ;
#4990 = CIRCLE ( 'NONE', #11816, 60.74260934110282051 ) ;
#4991 = ORIENTED_EDGE ( 'NONE', *, *, #10034, .F. ) ;
#4992 = DIRECTION ( 'NONE',  ( 6.982962677686266711E-15, -0.000000000000000000, 1.000000000000000000 ) ) ;
#4993 = EDGE_CURVE ( 'NONE', #11573, #6558, #8920, .T. ) ;
#4994 = DIRECTION ( 'NONE',  ( 0.3427509529624095941, 0.9394263059140722794, -0.000000000000000000 ) ) ;
#4995 = DIRECTION ( 'NONE',  ( -0.8830229359480288309, -0.4693298356057531984, 0.000000000000000000 ) ) ;
#4996 = CYLINDRICAL_SURFACE ( 'NONE', #13636, 42.50000000000000000 ) ;
#4997 = ORIENTED_EDGE ( 'NONE', *, *, #12081, .F. ) ;
#4998 = AXIS2_PLACEMENT_3D ( 'NONE', #19557, #8710, #15148 ) ;
#4999 = CARTESIAN_POINT ( 'NONE',  ( -130.9868171408399462, -91.88282611735539263, -10.00000000000000355 ) ) ;
#5000 = DIRECTION ( 'NONE',  ( -0.000000000000000000, -0.000000000000000000, -1.000000000000000000 ) ) ;
#5001 = AXIS2_PLACEMENT_3D ( 'NONE', #2064, #5036, #12688 ) ;
#5002 = ORIENTED_EDGE ( 'NONE', *, *, #19119, .T. ) ;
#5003 = CYLINDRICAL_SURFACE ( 'NONE', #17225, 62.91752772691707207 ) ;
#5004 = LINE ( 'NONE', #4696, #6510 ) ;
#5005 = DIRECTION ( 'NONE',  ( -1.000000000000000000, 0.000000000000000000, 0.000000000000000000 ) ) ;
#5006 = CARTESIAN_POINT ( 'NONE',  ( -23.23469325536272478, -13.41455640552162443, 14.88498244535561454 ) ) ;
#5007 = EDGE_CURVE ( 'NONE', #16722, #3030, #18028, .T. ) ;
#5008 = VECTOR ( 'NONE', #18332, 1000.000000000000000 ) ;
#5009 = VECTOR ( 'NONE', #19865, 1000.000000000000000 ) ;
#5010 = DIRECTION ( 'NONE',  ( -1.000000000000000000, 0.000000000000000000, 0.000000000000000000 ) ) ;
#5011 = CARTESIAN_POINT ( 'NONE',  ( -159.9599531637108782, -36.50981547337168109, 39.99999999999999289 ) ) ;
#5012 = CARTESIAN_POINT ( 'NONE',  ( -75.49180387445471752, 117.9024752767885786, -0.8621022543900443980 ) ) ;
#5013 = EDGE_LOOP ( 'NONE', ( #16850, #19899, #1456, #18040 ) ) ;
#5014 = EDGE_CURVE ( 'NONE', #17034, #1059, #9596, .T. ) ;
#5015 = DIRECTION ( 'NONE',  ( -1.000000000000000000, 0.000000000000000000, 0.000000000000000000 ) ) ;
#5016 = EDGE_LOOP ( 'NONE', ( #17162, #10017, #17921, #12194 ) ) ;
#5017 = VECTOR ( 'NONE', #16848, 1000.000000000000000 ) ;
#5018 = ORIENTED_EDGE ( 'NONE', *, *, #5379, .T. ) ;
#5019 = ORIENTED_EDGE ( 'NONE', *, *, #19885, .T. ) ;
#5020 = DIRECTION ( 'NONE',  ( -0.000000000000000000, -0.000000000000000000, 1.000000000000000000 ) ) ;
#5021 = EDGE_CURVE ( 'NONE', #7664, #14568, #7962, .T. ) ;
#5022 = FACE_BOUND ( 'NONE', #13984, .T. ) ;
#5023 = AXIS2_PLACEMENT_3D ( 'NONE', #18720, #4703, #9604 ) ;
#5024 = ORIENTED_EDGE ( 'NONE', *, *, #12344, .F. ) ;
#5025 = VECTOR ( 'NONE', #15688, 1000.000000000000227 ) ;
#5026 = CARTESIAN_POINT ( 'NONE',  ( 159.9599531637113330, -36.50981547336952104, 39.99999999999999289 ) ) ;
#5027 = DIRECTION ( 'NONE',  ( 0.000000000000000000, 0.000000000000000000, -1.000000000000000000 ) ) ;
#5028 = DIRECTION ( 'NONE',  ( 1.000000000000000000, 0.000000000000000000, -6.994638739193269649E-15 ) ) ;
#5029 = VECTOR ( 'NONE', #15784, 999.9999999999998863 ) ;
#5030 = DIRECTION ( 'NONE',  ( 0.000000000000000000, 0.000000000000000000, 1.000000000000000000 ) ) ;
#5031 = DIRECTION ( 'NONE',  ( 1.000000000000000000, 0.000000000000000000, 0.000000000000000000 ) ) ;
#5032 = VERTEX_POINT ( 'NONE', #393 ) ;
#5033 = CARTESIAN_POINT ( 'NONE',  ( -5.111158570922238020, 2.605298826210300511, 283.5832628385307999 ) ) ;
#5034 = AXIS2_PLACEMENT_3D ( 'NONE', #509, #14521, #6655 ) ;
#5035 = EDGE_CURVE ( 'NONE', #6926, #6009, #17292, .T. ) ;
#5036 = DIRECTION ( 'NONE',  ( -0.000000000000000000, -0.000000000000000000, -1.000000000000000000 ) ) ;
#5037 = CARTESIAN_POINT ( 'NONE',  ( 103.8725996235405518, -124.7053175801592602, 39.32360563185468294 ) ) ;
#5038 = ORIENTED_EDGE ( 'NONE', *, *, #10505, .F. ) ;
#5039 = ADVANCED_FACE ( 'NONE', ( #3269 ), #1725, .F. ) ;
#5040 = LINE ( 'NONE', #422, #3541 ) ;
#5041 = CARTESIAN_POINT ( 'NONE',  ( -70.05487284751588106, 132.6360328284314392, 7.773882658412580859 ) ) ;
#5042 = AXIS2_PLACEMENT_3D ( 'NONE', #2237, #8664, #11537 ) ;
#5043 = ORIENTED_EDGE ( 'NONE', *, *, #4376, .F. ) ;
#5044 = ORIENTED_EDGE ( 'NONE', *, *, #3382, .F. ) ;
#5045 = VERTEX_POINT ( 'NONE', #191 ) ;
#5046 = APPLICATION_PROTOCOL_DEFINITION ( 'draft international standard', 'automotive_design', 1998, #17190 ) ;
#5047 = CIRCLE ( 'NONE', #4040, 112.8770930172170210 ) ;
#5048 = ORIENTED_EDGE ( 'NONE', *, *, #6968, .T. ) ;
#5049 = CARTESIAN_POINT ( 'NONE',  ( 39.84224160888901167, 67.36461649554546227, 248.9926560891072143 ) ) ;
#5050 = EDGE_CURVE ( 'NONE', #4182, #4447, #766, .T. ) ;
#5051 = CARTESIAN_POINT ( 'NONE',  ( -149.7511488714461620, 8.920208118124556051, 9.601641421770001017 ) ) ;
#5052 = ADVANCED_FACE ( 'NONE', ( #499 ), #6743, .T. ) ;
#5053 = STYLED_ITEM ( 'NONE', ( #2645 ), #1054 ) ;
#5054 = VERTEX_POINT ( 'NONE', #15850 ) ;
#5055 = DIRECTION ( 'NONE',  ( -0.6427876096865353661, -0.7660444431189813441, 0.000000000000000000 ) ) ;
#5056 = LINE ( 'NONE', #13099, #18438 ) ;
#5057 = DIRECTION ( 'NONE',  ( -6.982962677686266711E-15, 0.000000000000000000, -1.000000000000000000 ) ) ;
#5058 = LINE ( 'NONE', #1773, #19937 ) ;
#5059 = DIRECTION ( 'NONE',  ( -1.000000000000000000, -0.000000000000000000, 0.000000000000000000 ) ) ;
#5060 = EDGE_CURVE ( 'NONE', #15899, #10298, #14314, .T. ) ;
#5061 = CIRCLE ( 'NONE', #799, 30.00000000000000000 ) ;
#5062 = CARTESIAN_POINT ( 'NONE',  ( -159.9599531637108782, -36.50981547337168109, 60.00000000000000000 ) ) ;
#5063 = CARTESIAN_POINT ( 'NONE',  ( -176.7850001792984926, -190.0000000000000284, 6.572490470375933036 ) ) ;
#5064 = FACE_OUTER_BOUND ( 'NONE', #11938, .T. ) ;
#5065 = ORIENTED_EDGE ( 'NONE', *, *, #135, .T. ) ;
#5066 = CARTESIAN_POINT ( 'NONE',  ( -117.6617105120774625, 62.20691784305332561, -29.20604482175252414 ) ) ;
#5067 = CIRCLE ( 'NONE', #17474, 106.4288957539801004 ) ;
#5068 = EDGE_CURVE ( 'NONE', #17628, #1213, #2728, .T. ) ;
#5069 = ORIENTED_EDGE ( 'NONE', *, *, #4754, .F. ) ;
#5070 = ORIENTED_EDGE ( 'NONE', *, *, #13129, .F. ) ;
#5071 = EDGE_LOOP ( 'NONE', ( #10394, #4569, #10823, #1559 ) ) ;
#5072 = DIRECTION ( 'NONE',  ( -6.982962677686266711E-15, 7.888609052210118054E-31, -1.000000000000000000 ) ) ;
#5073 = CARTESIAN_POINT ( 'NONE',  ( -63.98537287693041264, 94.20918150411493741, 14.88498244535589876 ) ) ;
#5074 = DIRECTION ( 'NONE',  ( 0.000000000000000000, 0.000000000000000000, 1.000000000000000000 ) ) ;
#5075 = DIRECTION ( 'NONE',  ( 0.4999999999999918954, -0.8660254037844431485, -3.520662956770156304E-15 ) ) ;
#5076 = DIRECTION ( 'NONE',  ( -0.2225209339563195554, 0.9749279121818223981, 0.000000000000000000 ) ) ;
#5077 = CARTESIAN_POINT ( 'NONE',  ( 1.678175111358129801, 5.485913980968024184, 293.5832628385307999 ) ) ;
#5078 = CARTESIAN_POINT ( 'NONE',  ( -59.51523122377252406, 12.14914984460740932, 283.5832628385307999 ) ) ;
#5079 = DIRECTION ( 'NONE',  ( 1.000000000000000000, 0.000000000000000000, -0.000000000000000000 ) ) ;
#5080 = CARTESIAN_POINT ( 'NONE',  ( 0.000000000000000000, 0.000000000000000000, 4.999999999999948486 ) ) ;
#5081 = CIRCLE ( 'NONE', #16506, 60.74260934110282051 ) ;
#5082 = CARTESIAN_POINT ( 'NONE',  ( 5.590028426173780929, 1.289614712049194534, 293.5832628385307999 ) ) ;
#5083 = VERTEX_POINT ( 'NONE', #19425 ) ;
#5084 = DIRECTION ( 'NONE',  ( 1.000000000000000000, 0.000000000000000000, -6.994638739193269649E-15 ) ) ;
#5085 = VECTOR ( 'NONE', #1265, 1000.000000000000000 ) ;
#5086 = CARTESIAN_POINT ( 'NONE',  ( 103.2967819461769921, 53.25886146954521649, 39.88498244535472992 ) ) ;
#5087 = ORIENTED_EDGE ( 'NONE', *, *, #2258, .T. ) ;
#5088 = ORIENTED_EDGE ( 'NONE', *, *, #19969, .F. ) ;
#5089 = ORIENTED_EDGE ( 'NONE', *, *, #6746, .T. ) ;
#5090 = ORIENTED_EDGE ( 'NONE', *, *, #16524, .F. ) ;
#5091 = CARTESIAN_POINT ( 'NONE',  ( -1.379293853801755176, 78.26059000578311498, 132.4711112102474146 ) ) ;
#5092 = PRODUCT_DEFINITION_SHAPE ( 'NONE', 'NONE',  #12261 ) ;
#5093 = ORIENTED_EDGE ( 'NONE', *, *, #15855, .T. ) ;
#5094 = LINE ( 'NONE', #3448, #211 ) ;
#5095 = AXIS2_PLACEMENT_3D ( 'NONE', #6586, #10045, #14245 ) ;
#5096 = CARTESIAN_POINT ( 'NONE',  ( -59.06449708980196078, -51.36153797460887915, 132.4711112102474146 ) ) ;
#5097 = SURFACE_STYLE_USAGE ( .BOTH. , #11114 ) ;
#5098 = DIRECTION ( 'NONE',  ( -0.000000000000000000, -0.000000000000000000, 1.000000000000000000 ) ) ;
#5099 = ORIENTED_EDGE ( 'NONE', *, *, #3637, .T. ) ;
#5100 = CARTESIAN_POINT ( 'NONE',  ( 123.6373235125731469, -84.94667440144652915, -10.00000000000000000 ) ) ;
#5101 = DIRECTION ( 'NONE',  ( -0.000000000000000000, -0.000000000000000000, 1.000000000000000000 ) ) ;
#5102 = ORIENTED_EDGE ( 'NONE', *, *, #18991, .T. ) ;
#5103 = CARTESIAN_POINT ( 'NONE',  ( -29.99999999999887379, 265.0000000000000000, 4.999999999999158007 ) ) ;
#5104 = CYLINDRICAL_SURFACE ( 'NONE', #11703, 60.74260934110282051 ) ;
#5105 = CIRCLE ( 'NONE', #2171, 3.224098631618460331 ) ;
#5106 = CARTESIAN_POINT ( 'NONE',  ( 7.350000000000000533, -10.39230484541326582, 0.000000000000000000 ) ) ;
#5107 = DIRECTION ( 'NONE',  ( -6.982962677686266711E-15, 0.000000000000000000, -1.000000000000000000 ) ) ;
#5108 = DIRECTION ( 'NONE',  ( -0.000000000000000000, -0.000000000000000000, 1.000000000000000000 ) ) ;
#5109 = VECTOR ( 'NONE', #20024, 1000.000000000000000 ) ;
#5110 = CARTESIAN_POINT ( 'NONE',  ( -74.99285178184982215, 118.2204394347531604, 5.472170298398729926 ) ) ;
#5111 = ORIENTED_EDGE ( 'NONE', *, *, #1942, .F. ) ;
#5112 = EDGE_CURVE ( 'NONE', #2560, #6500, #11814, .T. ) ;
#5113 = CYLINDRICAL_SURFACE ( 'NONE', #14164, 7.500000000000003553 ) ;
#5114 = VERTEX_POINT ( 'NONE', #985 ) ;
#5115 = ORIENTED_EDGE ( 'NONE', *, *, #3022, .F. ) ;
#5116 = DIRECTION ( 'NONE',  ( 0.000000000000000000, 0.000000000000000000, 1.000000000000000000 ) ) ;
#5117 = ORIENTED_EDGE ( 'NONE', *, *, #17857, .F. ) ;
#5118 = AXIS2_PLACEMENT_3D ( 'NONE', #15478, #9128, #1464 ) ;
#5119 = LINE ( 'NONE', #507, #14328 ) ;
#5120 = VECTOR ( 'NONE', #6069, 1000.000000000000227 ) ;
#5121 = EDGE_CURVE ( 'NONE', #10879, #7170, #1418, .T. ) ;
#5122 = CARTESIAN_POINT ( 'NONE',  ( 60.08331549348424971, 8.939227532413909216, 293.5832628385307999 ) ) ;
#5123 = ORIENTED_EDGE ( 'NONE', *, *, #6895, .T. ) ;
#5124 = EDGE_CURVE ( 'NONE', #11258, #7556, #3670, .T. ) ;
#5125 = CARTESIAN_POINT ( 'NONE',  ( 163.5019688434126977, -20.99123081650019529, 39.99999999999999289 ) ) ;
#5126 = DIRECTION ( 'NONE',  ( 1.000000000000000000, 0.000000000000000000, 0.000000000000000000 ) ) ;
#5127 = EDGE_CURVE ( 'NONE', #12537, #15505, #10293, .T. ) ;
#5128 = DIRECTION ( 'NONE',  ( 0.000000000000000000, 0.000000000000000000, -1.000000000000000000 ) ) ;
#5129 = VECTOR ( 'NONE', #2935, 1000.000000000000000 ) ;
#5130 = LINE ( 'NONE', #17606, #6174 ) ;
#5131 = DIRECTION ( 'NONE',  ( -0.000000000000000000, -0.000000000000000000, 1.000000000000000000 ) ) ;
#5132 = CARTESIAN_POINT ( 'NONE',  ( 110.0000000000000142, 0.000000000000000000, -9.999999999999994671 ) ) ;
#5133 = VERTEX_POINT ( 'NONE', #18081 ) ;
#5134 = FACE_OUTER_BOUND ( 'NONE', #8850, .T. ) ;
#5135 = DIRECTION ( 'NONE',  ( 0.3420201433256757073, -0.9396926207859057634, 0.000000000000000000 ) ) ;
#5136 = LINE ( 'NONE', #11360, #14057 ) ;
#5137 = CARTESIAN_POINT ( 'NONE',  ( 98.08728810296497613, -113.5042871117747865, 38.12342019507656232 ) ) ;
#5138 = AXIS2_PLACEMENT_3D ( 'NONE', #2428, #4150, #8656 ) ;
#5139 = ORIENTED_EDGE ( 'NONE', *, *, #13851, .T. ) ;
#5140 = EDGE_CURVE ( 'NONE', #11666, #14566, #2434, .T. ) ;
#5141 = CIRCLE ( 'NONE', #2198, 9.000000000000001776 ) ;
#5142 = DIRECTION ( 'NONE',  ( -0.000000000000000000, -1.000000000000000000, -0.000000000000000000 ) ) ;
#5143 = DIRECTION ( 'NONE',  ( 1.000000000000000000, 0.000000000000000000, 0.000000000000000000 ) ) ;
#5144 = ORIENTED_EDGE ( 'NONE', *, *, #3668, .T. ) ;
#5145 = ORIENTED_EDGE ( 'NONE', *, *, #4118, .T. ) ;
#5147 = VERTEX_POINT ( 'NONE', #2336 ) ;
#5146 = CIRCLE ( 'NONE', #14930, 15.91767397667354800 ) ;
#5148 = ITEM_DEFINED_TRANSFORMATION ( 'NONE', 'NONE', #8818,  #18639 ) ;
#5149 = EDGE_LOOP ( 'NONE', ( #19102, #15112, #4777, #11521 ) ) ;
#5150 = FACE_OUTER_BOUND ( 'NONE', #1908, .T. ) ;
#5151 = CARTESIAN_POINT ( 'NONE',  ( -132.7010181243791465, 70.09019636137327325, 38.03942095735952478 ) ) ;
#5152 = VERTEX_POINT ( 'NONE', #9906 ) ;
#5153 = EDGE_CURVE ( 'NONE', #5943, #7173, #3958, .T. ) ;
#5154 = CARTESIAN_POINT ( 'NONE',  ( 133.2435246741110006, -68.89240257401093004, 40.00000000000000000 ) ) ;
#5155 = CARTESIAN_POINT ( 'NONE',  ( -92.41621553527373578, -118.1510961661445407, -7.909716053491956167 ) ) ;
#5156 = EDGE_CURVE ( 'NONE', #7528, #20089, #8278, .T. ) ;
#5157 = CARTESIAN_POINT ( 'NONE',  ( 0.000000000000000000, 0.000000000000000000, -100.0000000000000000 ) ) ;
#5158 = CARTESIAN_POINT ( 'NONE',  ( 50.93469132750264095, 59.42266395395811429, 110.7293897666001214 ) ) ;
#5159 = FACE_OUTER_BOUND ( 'NONE', #12209, .T. ) ;
#5160 = CIRCLE ( 'NONE', #19199, 7.500000000000020428 ) ;
#5161 = DIRECTION ( 'NONE',  ( -0.1736481776669306920, 0.9848077530122080203, 0.000000000000000000 ) ) ;
#5162 = CARTESIAN_POINT ( 'NONE',  ( 0.000000000000000000, 0.000000000000000000, 4.999999999999948486 ) ) ;
#5163 = DIRECTION ( 'NONE',  ( -0.000000000000000000, -0.000000000000000000, -1.000000000000000000 ) ) ;
#5164 = DIRECTION ( 'NONE',  ( 0.000000000000000000, 0.000000000000000000, -1.000000000000000000 ) ) ;
#5165 = EDGE_LOOP ( 'NONE', ( #7138, #8339, #15488, #6548 ) ) ;
#5166 = EDGE_CURVE ( 'NONE', #11868, #8819, #3376, .T. ) ;
#5167 = CARTESIAN_POINT ( 'NONE',  ( -126.3908400843113924, 48.63710208285993275, -25.92855131512484590 ) ) ;
#5168 = ORIENTED_EDGE ( 'NONE', *, *, #6355, .F. ) ;
#5169 = VECTOR ( 'NONE', #2950, 1000.000000000000114 ) ;
#5170 = EDGE_LOOP ( 'NONE', ( #117, #2587, #2839, #14519, #9757, #16747 ) ) ;
#5171 = AXIS2_PLACEMENT_3D ( 'NONE', #11864, #16594, #2580 ) ;
#5172 = ORIENTED_EDGE ( 'NONE', *, *, #2992, .T. ) ;
#5173 = EDGE_CURVE ( 'NONE', #16123, #4193, #15691, .T. ) ;
#5174 = DIRECTION ( 'NONE',  ( -0.000000000000000000, -0.000000000000000000, 1.000000000000000000 ) ) ;
#5175 = EDGE_CURVE ( 'NONE', #10874, #7342, #13830, .T. ) ;
#5176 = CARTESIAN_POINT ( 'NONE',  ( -134.9931224044436249, -65.39776452395025785, 7.096802314759633745 ) ) ;
#5177 = CARTESIAN_POINT ( 'NONE',  ( 57.61627707419551570, 19.23614321207255884, 283.5832628385307999 ) ) ;
#5178 = DIRECTION ( 'NONE',  ( 1.000000000000000000, 0.000000000000000000, 0.000000000000000000 ) ) ;
#5179 = EDGE_CURVE ( 'NONE', #16678, #4193, #885, .T. ) ;
#5180 = DIRECTION ( 'NONE',  ( 0.000000000000000000, 0.000000000000000000, 1.000000000000000000 ) ) ;
#5181 = DIRECTION ( 'NONE',  ( -0.9749279121818255067, 0.2225209339563057331, 0.000000000000000000 ) ) ;
#5182 = LINE ( 'NONE', #13036, #13353 ) ;
#5183 = CARTESIAN_POINT ( 'NONE',  ( 7.950000000000000178, -10.39230484541326582, 0.000000000000000000 ) ) ;
#5184 = CARTESIAN_POINT ( 'NONE',  ( -78.26059000578311498, -1.379293853802032732, 132.4711112102474146 ) ) ;
#5185 = ORIENTED_EDGE ( 'NONE', *, *, #12025, .T. ) ;
#5186 = CIRCLE ( 'NONE', #6816, 15.91767397667354444 ) ;
#5187 = DIRECTION ( 'NONE',  ( -0.1736481776669280275, 0.9848077530122084644, 2.152196535136391663E-15 ) ) ;
#5188 = EDGE_LOOP ( 'NONE', ( #7994, #10340, #14731, #298 ) ) ;
#5189 = ORIENTED_EDGE ( 'NONE', *, *, #12912, .F. ) ;
#5190 = ORIENTED_EDGE ( 'NONE', *, *, #9146, .F. ) ;
#5191 = ORIENTED_EDGE ( 'NONE', *, *, #3870, .F. ) ;
#5192 = EDGE_LOOP ( 'NONE', ( #10183, #18156 ) ) ;
#5193 = DIRECTION ( 'NONE',  ( -0.7660444431189707970, -0.6427876096865481337, -0.000000000000000000 ) ) ;
#5194 = AXIS2_PLACEMENT_3D ( 'NONE', #16979, #4600, #12262 ) ;
#5195 = CIRCLE ( 'NONE', #20202, 60.74260934110282051 ) ;
#5196 = DIRECTION ( 'NONE',  ( 1.000000000000000000, 0.000000000000000000, 0.000000000000000000 ) ) ;
#5197 = CIRCLE ( 'NONE', #14001, 15.91767397667354089 ) ;
#5198 = FACE_BOUND ( 'NONE', #17469, .T. ) ;
#5199 = CARTESIAN_POINT ( 'NONE',  ( -39.80940113485987553, 48.72193424476490975, 132.4711112102474146 ) ) ;
#5200 = EDGE_LOOP ( 'NONE', ( #19349, #5514, #15572, #1436 ) ) ;
#5201 = CARTESIAN_POINT ( 'NONE',  ( 130.7962991791399077, -73.43504534872144518, -5.497766754562231739 ) ) ;
#5202 = DIRECTION ( 'NONE',  ( 0.000000000000000000, 0.000000000000000000, 1.000000000000000000 ) ) ;
#5203 = ORIENTED_EDGE ( 'NONE', *, *, #18109, .F. ) ;
#5204 = DIRECTION ( 'NONE',  ( 0.2225209339563194721, -0.9749279121818225091, 0.000000000000000000 ) ) ;
#5205 = FACE_OUTER_BOUND ( 'NONE', #9961, .T. ) ;
#5206 = DIRECTION ( 'NONE',  ( -0.000000000000000000, -0.000000000000000000, 1.000000000000000000 ) ) ;
#5207 = CARTESIAN_POINT ( 'NONE',  ( 60.47951622432751151, 49.67518383744852883, 110.7293897666001214 ) ) ;
#5208 = DIRECTION ( 'NONE',  ( 0.000000000000000000, -0.5000000000000009992, 0.8660254037844380415 ) ) ;
#5209 = DIRECTION ( 'NONE',  ( -0.000000000000000000, -0.000000000000000000, -1.000000000000000000 ) ) ;
#5210 = CARTESIAN_POINT ( 'NONE',  ( 83.21341172527402819, -124.8022162803316348, 37.02557696701107659 ) ) ;
#5211 = VECTOR ( 'NONE', #16139, 1000.000000000000000 ) ;
#5212 = EDGE_LOOP ( 'NONE', ( #921, #1087, #18578, #16287 ) ) ;
#5213 = AXIS2_PLACEMENT_3D ( 'NONE', #10660, #10451, #15374 ) ;
#5214 = DIRECTION ( 'NONE',  ( 1.000000000000000000, 0.000000000000000000, 0.000000000000000000 ) ) ;
#5215 = ORIENTED_EDGE ( 'NONE', *, *, #19520, .F. ) ;
#5216 = ORIENTED_EDGE ( 'NONE', *, *, #13359, .T. ) ;
#5217 = CYLINDRICAL_SURFACE ( 'NONE', #8588, 62.91752772691707207 ) ;
#5218 = VERTEX_POINT ( 'NONE', #17697 ) ;
#5219 = CARTESIAN_POINT ( 'NONE',  ( 47.29944656917759005, 41.48948842197133757, 132.4711112102474146 ) ) ;
#5220 = B_SPLINE_CURVE_WITH_KNOTS ( 'NONE', 3,
 ( #8968, #4584, #10708, #16962, #15210, #12341, #2953, #18397 ),
 .UNSPECIFIED., .F., .F.,
 ( 4, 2, 2, 4 ),
 ( 0.005257893453559907108, 0.006567392922673239916, 0.007876892391786571856, 0.01049589133001323747 ),
 .UNSPECIFIED. ) ;
#5221 = FACE_OUTER_BOUND ( 'NONE', #15178, .T. ) ;
#5222 = CARTESIAN_POINT ( 'NONE',  ( 0.09252763182292003674, -8.674330214978045461, -2.975619346028160805 ) ) ;
#5223 = CARTESIAN_POINT ( 'NONE',  ( 17.50000000000001776, 2.143131898507868643E-15, 60.00000000000000000 ) ) ;
#5224 = VECTOR ( 'NONE', #17822, 1000.000000000000000 ) ;
#5225 = AXIS2_PLACEMENT_3D ( 'NONE', #3329, #16114, #5178 ) ;
#5226 = EDGE_CURVE ( 'NONE', #8307, #4702, #5500, .T. ) ;
#5227 = FACE_OUTER_BOUND ( 'NONE', #1962, .T. ) ;
#5228 = CARTESIAN_POINT ( 'NONE',  ( -15.91767397667354800, 164.0736214083062805, 60.00000000000000000 ) ) ;
#5229 = CARTESIAN_POINT ( 'NONE',  ( 100.6969204557048414, -129.5542747642291772, 2.663644724477163717 ) ) ;
#5230 = DIRECTION ( 'NONE',  ( -0.9848077530122085754, 0.1736481776669273336, 0.000000000000000000 ) ) ;
#5231 = DIRECTION ( 'NONE',  ( -0.000000000000000000, -0.000000000000000000, 1.000000000000000000 ) ) ;
#5232 = FACE_OUTER_BOUND ( 'NONE', #10753, .T. ) ;
#5233 = CARTESIAN_POINT ( 'NONE',  ( 0.000000000000000000, 0.000000000000000000, 49.99999999999999289 ) ) ;
#5234 = CARTESIAN_POINT ( 'NONE',  ( 59.39925916207545242, 20.74471755083624203, 132.4711112102474146 ) ) ;
#5235 = CARTESIAN_POINT ( 'NONE',  ( -57.65577537092151772, 11.00103590902930328, 112.0427633081292385 ) ) ;
#5236 = ORIENTED_EDGE ( 'NONE', *, *, #12545, .T. ) ;
#5237 = EDGE_CURVE ( 'NONE', #10908, #301, #11224, .T. ) ;
#5238 = CARTESIAN_POINT ( 'NONE',  ( 0.000000000000000000, 0.000000000000000000, -110.0000000000000000 ) ) ;
#5239 = CARTESIAN_POINT ( 'NONE',  ( -102.9658523914788617, 109.0818325198187893, 44.38238497178959108 ) ) ;
#5240 = ORIENTED_EDGE ( 'NONE', *, *, #7603, .T. ) ;
#5241 = ORIENTED_EDGE ( 'NONE', *, *, #11091, .F. ) ;
#5242 = EDGE_CURVE ( 'NONE', #14660, #15773, #2410, .T. ) ;
#5243 = ORIENTED_EDGE ( 'NONE', *, *, #548, .F. ) ;
#5244 = ORIENTED_EDGE ( 'NONE', *, *, #13903, .F. ) ;
#5245 = CARTESIAN_POINT ( 'NONE',  ( -15.91767397667354800, 141.9028892025177413, 39.99999999999999289 ) ) ;
#5246 = ORIENTED_EDGE ( 'NONE', *, *, #3143, .T. ) ;
#5247 = DIRECTION ( 'NONE',  ( -0.9848077530122062440, -0.1736481776669404620, -0.000000000000000000 ) ) ;
#5248 = PLANE ( 'NONE',  #16148 ) ;
#5249 = CARTESIAN_POINT ( 'NONE',  ( -99.98138848894345188, -130.5820681961508853, 3.371015809596708657 ) ) ;
#5250 = ORIENTED_EDGE ( 'NONE', *, *, #7228, .T. ) ;
#5251 = EDGE_CURVE ( 'NONE', #12873, #10598, #2140, .T. ) ;
#5252 = AXIS2_PLACEMENT_3D ( 'NONE', #15360, #7578, #16901 ) ;
#5253 = VECTOR ( 'NONE', #2978, 1000.000000000000000 ) ;
#5254 = CARTESIAN_POINT ( 'NONE',  ( -63.98537287693041264, 94.20918150411493741, 14.88498244535589876 ) ) ;
#5255 = CARTESIAN_POINT ( 'NONE',  ( 0.000000000000000000, 0.000000000000000000, -10.00000000000000178 ) ) ;
#5256 = PLANE ( 'NONE',  #1352 ) ;
#5257 = CARTESIAN_POINT ( 'NONE',  ( -27.10287801637868199, 1.507547295587424951, 14.88498244535564297 ) ) ;
#5258 = LINE ( 'NONE', #1987, #14555 ) ;
#5259 = ORIENTED_EDGE ( 'NONE', *, *, #19589, .T. ) ;
#5260 = ADVANCED_FACE ( 'NONE', ( #10004 ), #14706, .T. ) ;
#5261 = DIRECTION ( 'NONE',  ( 0.000000000000000000, -0.5000000000000009992, 0.8660254037844380415 ) ) ;
#5262 = EDGE_CURVE ( 'NONE', #14061, #11180, #6005, .T. ) ;
#5263 = ADVANCED_FACE ( 'NONE', ( #11917 ), #3140, .T. ) ;
#5264 = ORIENTED_EDGE ( 'NONE', *, *, #18361, .F. ) ;
#5265 = ORIENTED_EDGE ( 'NONE', *, *, #16057, .F. ) ;
#5266 = ORIENTED_EDGE ( 'NONE', *, *, #1033, .T. ) ;
#5267 = CARTESIAN_POINT ( 'NONE',  ( 70.38703763562273252, -92.47916748300480094, 14.88498244535495907 ) ) ;
#5268 = ADVANCED_FACE ( 'NONE', ( #12230 ), #5700, .T. ) ;
#5269 = CARTESIAN_POINT ( 'NONE',  ( 54.67896814532641514, 21.36933070621782349, 111.4180192758973362 ) ) ;
#5270 = DIRECTION ( 'NONE',  ( -0.9781142164131917394, 0.2080686897406911207, 0.000000000000000000 ) ) ;
#5271 = LINE ( 'NONE', #12930, #14031 ) ;
#5272 = ORIENTED_EDGE ( 'NONE', *, *, #17501, .F. ) ;
#5273 = FACE_OUTER_BOUND ( 'NONE', #6023, .T. ) ;
#5274 = CARTESIAN_POINT ( 'NONE',  ( -133.3574802752804658, -81.67441013338864764, 1.778968245714176666 ) ) ;
#5275 = AXIS2_PLACEMENT_3D ( 'NONE', #13445, #5695, #13964 ) ;
#5276 = CARTESIAN_POINT ( 'NONE',  ( -86.01343624116279329, 31.38211805825948630, 40.00000000000000000 ) ) ;
#5277 = CARTESIAN_POINT ( 'NONE',  ( 0.000000000000000000, 0.000000000000000000, 283.5832628385307999 ) ) ;
#5278 = CARTESIAN_POINT ( 'NONE',  ( 97.83161216922243852, -133.5187961265288266, 32.56398726576716740 ) ) ;
#5279 = VECTOR ( 'NONE', #7699, 1000.000000000000000 ) ;
#5280 = CARTESIAN_POINT ( 'NONE',  ( -4.811834253408968642, -3.123743752084039205, 293.5832628385307999 ) ) ;
#5281 = EDGE_LOOP ( 'NONE', ( #14805, #992, #6577, #17055 ) ) ;
#5282 = EDGE_CURVE ( 'NONE', #5083, #3700, #7694, .T. ) ;
#5283 = ADVANCED_FACE ( 'NONE', ( #16649 ), #18382, .T. ) ;
#5284 = ORIENTED_EDGE ( 'NONE', *, *, #1273, .T. ) ;
#5285 = EDGE_CURVE ( 'NONE', #17930, #9086, #18482, .T. ) ;
#5286 = EDGE_CURVE ( 'NONE', #3620, #16612, #8955, .T. ) ;
#5287 = VERTEX_POINT ( 'NONE', #6010 ) ;
#5288 = ORIENTED_EDGE ( 'NONE', *, *, #9531, .F. ) ;
#5289 = VERTEX_POINT ( 'NONE', #1398 ) ;
#5290 = LINE ( 'NONE', #11513, #19704 ) ;
#5291 = ORIENTED_EDGE ( 'NONE', *, *, #12661, .T. ) ;
#5292 = CARTESIAN_POINT ( 'NONE',  ( -41.48948842197086861, 47.29944656917800216, 248.9926560891072143 ) ) ;
#5293 = LINE ( 'NONE', #774, #14513 ) ;
#5294 = CARTESIAN_POINT ( 'NONE',  ( 26.85905058935160383, 1.464553941565464035, 39.88498244535526283 ) ) ;
#5295 = EDGE_LOOP ( 'NONE', ( #1030, #11317, #13331 ) ) ;
#5296 = FACE_OUTER_BOUND ( 'NONE', #15970, .T. ) ;
#5297 = DIRECTION ( 'NONE',  ( -0.1736481776669280275, 0.9848077530122084644, 2.152196535136391663E-15 ) ) ;
#5298 = EDGE_LOOP ( 'NONE', ( #1751, #11217, #9202 ) ) ;
#5299 = CARTESIAN_POINT ( 'NONE',  ( -107.4999999999999716, -200.0000000000000000, 10.00000000000000178 ) ) ;
#5300 = DIRECTION ( 'NONE',  ( 1.000000000000000000, 0.000000000000000000, 0.000000000000000000 ) ) ;
#5301 = LINE ( 'NONE', #14701, #7873 ) ;
#5302 = EDGE_CURVE ( 'NONE', #16902, #7679, #2634, .T. ) ;
#5303 = CARTESIAN_POINT ( 'NONE',  ( -138.7698490687724586, -23.27885928005511218, -14.95860281343817633 ) ) ;
#5304 = DIRECTION ( 'NONE',  ( -1.000000000000000000, 0.000000000000000000, 0.000000000000000000 ) ) ;
#5305 = DIRECTION ( 'NONE',  ( 0.000000000000000000, 0.000000000000000000, -1.000000000000000000 ) ) ;
#5306 = ORIENTED_EDGE ( 'NONE', *, *, #6535, .T. ) ;
#5307 = CARTESIAN_POINT ( 'NONE',  ( -1.067261513540418057E-16, -0.8794428697894906000, -9.000000000000000000 ) ) ;
#5308 = CIRCLE ( 'NONE', #16727, 34.99999999999997868 ) ;
#5309 = ORIENTED_EDGE ( 'NONE', *, *, #10759, .F. ) ;
#5310 = EDGE_CURVE ( 'NONE', #6137, #13930, #16824, .T. ) ;
#5311 = VERTEX_POINT ( 'NONE', #12124 ) ;
#5312 = DIRECTION ( 'NONE',  ( 0.000000000000000000, 0.000000000000000000, -1.000000000000000000 ) ) ;
#5313 = VERTEX_POINT ( 'NONE', #13556 ) ;
#5314 = PLANE ( 'NONE',  #7137 ) ;
#5315 = CARTESIAN_POINT ( 'NONE',  ( -91.69207598197974107, -118.7138234487252930, 47.50433883429951720 ) ) ;
#5316 = CARTESIAN_POINT ( 'NONE',  ( -7.500000000000008882, 164.0736214083062805, 60.00000000000000000 ) ) ;
#5317 = VERTEX_POINT ( 'NONE', #10695 ) ;
#5318 = CARTESIAN_POINT ( 'NONE',  ( -78.68887634719366986, -147.8252249328922687, 39.99999999999999289 ) ) ;
#5320 = AXIS2_PLACEMENT_3D ( 'NONE', #8262, #8933, #8463 ) ;
#5319 = CARTESIAN_POINT ( 'NONE',  ( 101.4288913641181864, -128.4806265586112488, 2.048058698311194803 ) ) ;
#5321 = CIRCLE ( 'NONE', #3027, 9.999999999999994671 ) ;
#5322 = DIRECTION ( 'NONE',  ( -0.2225209339563047894, -0.9749279121818258398, 0.000000000000000000 ) ) ;
#5323 = DIRECTION ( 'NONE',  ( -0.000000000000000000, -0.000000000000000000, -1.000000000000000000 ) ) ;
#5324 = EDGE_LOOP ( 'NONE', ( #10540, #15253, #1165, #4889 ) ) ;
#5325 = DIRECTION ( 'NONE',  ( -1.000000000000000000, -1.047444401652940164E-14, 0.000000000000000000 ) ) ;
#5326 = FACE_OUTER_BOUND ( 'NONE', #1402, .T. ) ;
#5327 = VECTOR ( 'NONE', #1852, 1000.000000000000000 ) ;
#5328 = DIRECTION ( 'NONE',  ( 0.000000000000000000, 0.000000000000000000, -1.000000000000000000 ) ) ;
#5329 = CARTESIAN_POINT ( 'NONE',  ( 100.7812500000000142, -111.0996833858562667, 50.00000000000000000 ) ) ;
#5330 = ORIENTED_EDGE ( 'NONE', *, *, #2154, .F. ) ;
#5331 = CARTESIAN_POINT ( 'NONE',  ( 0.000000000000000000, 0.000000000000000000, 283.5832628385307999 ) ) ;
#5332 = CARTESIAN_POINT ( 'NONE',  ( -52.50000000000000000, -2.094888803305880013E-13, -115.0000000000000000 ) ) ;
#5333 = EDGE_LOOP ( 'NONE', ( #1433, #15130, #11920, #17618 ) ) ;
#5334 = ORIENTED_EDGE ( 'NONE', *, *, #11927, .T. ) ;
#5335 = ORIENTED_EDGE ( 'NONE', *, *, #16859, .F. ) ;
#5336 = CONTEXT_DEPENDENT_SHAPE_REPRESENTATION ( #7759, #18634 ) ;
#5337 = CIRCLE ( 'NONE', #428, 106.4288957539801288 ) ;
#5338 = AXIS2_PLACEMENT_3D ( 'NONE', #17679, #13724, #13048 ) ;
#5339 = ORIENTED_EDGE ( 'NONE', *, *, #9253, .F. ) ;
#5340 = CARTESIAN_POINT ( 'NONE',  ( 0.000000000000000000, 0.000000000000000000, 283.5832628385307999 ) ) ;
#5341 = CARTESIAN_POINT ( 'NONE',  ( 38.41834839689379777, -68.18670162478818497, 132.4711112102474146 ) ) ;
#5342 = ORIENTED_EDGE ( 'NONE', *, *, #19975, .T. ) ;
#5343 = AXIS2_PLACEMENT_3D ( 'NONE', #503, #795, #14710 ) ;
#5344 = CARTESIAN_POINT ( 'NONE',  ( 57.94128254008182921, 9.381844291199925578, 248.9926560891072143 ) ) ;
#5345 = DIRECTION ( 'NONE',  ( 1.000000000000000000, 0.000000000000000000, 0.000000000000000000 ) ) ;
#5346 = CARTESIAN_POINT ( 'NONE',  ( -95.64785785032820797, -115.7351073149044822, 5.855624241335786628 ) ) ;
#5347 = ORIENTED_EDGE ( 'NONE', *, *, #13140, .F. ) ;
#5348 = VECTOR ( 'NONE', #4818, 1000.000000000000000 ) ;
#5349 = LINE ( 'NONE', #13011, #18313 ) ;
#5350 = CARTESIAN_POINT ( 'NONE',  ( 19.23677882349201695, -57.61823435390814296, 283.5832628385307999 ) ) ;
#5351 = VECTOR ( 'NONE', #8564, 1000.000000000000000 ) ;
#5352 = LINE ( 'NONE', #17936, #14430 ) ;
#5353 = LINE ( 'NONE', #5448, #14356 ) ;
#5354 = FACE_OUTER_BOUND ( 'NONE', #18962, .T. ) ;
#5355 = ORIENTED_EDGE ( 'NONE', *, *, #19608, .F. ) ;
#5356 = DIRECTION ( 'NONE',  ( -0.000000000000000000, -0.000000000000000000, 1.000000000000000000 ) ) ;
#5357 = AXIS2_PLACEMENT_3D ( 'NONE', #12824, #19085, #10254 ) ;
#5358 = EDGE_CURVE ( 'NONE', #2409, #8834, #10303, .T. ) ;
#5359 =( GEOMETRIC_REPRESENTATION_CONTEXT ( 3 ) GLOBAL_UNCERTAINTY_ASSIGNED_CONTEXT ( ( #13552 ) ) GLOBAL_UNIT_ASSIGNED_CONTEXT ( ( #4370, #9071, #7539 ) ) REPRESENTATION_CONTEXT ( 'NONE', 'WORKASPACE' ) );
#5360 = VERTEX_POINT ( 'NONE', #5802 ) ;
#5361 = VERTEX_POINT ( 'NONE', #2837 ) ;
#5362 = EDGE_CURVE ( 'NONE', #14667, #10450, #3459, .T. ) ;
#5363 = DIRECTION ( 'NONE',  ( 0.9396926207859112035, 0.3420201433256609969, -6.456589605409174593E-15 ) ) ;
#5364 = LINE ( 'NONE', #9761, #2435 ) ;
#5365 = EDGE_CURVE ( 'NONE', #4682, #11852, #7629, .T. ) ;
#5366 = CARTESIAN_POINT ( 'NONE',  ( -48.72193424476477475, -39.80940113486002474, 248.9926560891072143 ) ) ;
#5367 = EDGE_CURVE ( 'NONE', #14347, #16722, #4102, .T. ) ;
#5368 = VECTOR ( 'NONE', #10046, 1000.000000000000227 ) ;
#5369 = LINE ( 'NONE', #17354, #3910 ) ;
#5370 = EDGE_LOOP ( 'NONE', ( #12508, #1431 ) ) ;
#5371 = EDGE_CURVE ( 'NONE', #7889, #11536, #17523, .T. ) ;
#5372 = DIRECTION ( 'NONE',  ( -0.1736481776669408228, -0.9848077530122062440, 1.076098267568195042E-15 ) ) ;
#5373 = CARTESIAN_POINT ( 'NONE',  ( -132.6415777375414393, -85.19230204982613941, 0.7648825228462121650 ) ) ;
#5374 = DIRECTION ( 'NONE',  ( -6.982962677686266711E-15, 0.000000000000000000, -1.000000000000000000 ) ) ;
#5375 = AXIS2_PLACEMENT_3D ( 'NONE', #10181, #577, #6826 ) ;
#5376 = CARTESIAN_POINT ( 'NONE',  ( 0.000000000000000000, 60.00000000000000000, -105.0000000000000142 ) ) ;
#5377 = CARTESIAN_POINT ( 'NONE',  ( -56.84754764479025368, -154.7316448359455308, 60.00000000000000000 ) ) ;
#5378 = ORIENTED_EDGE ( 'NONE', *, *, #10581, .T. ) ;
#5379 = EDGE_CURVE ( 'NONE', #17491, #13285, #18049, .T. ) ;
#5380 = ORIENTED_EDGE ( 'NONE', *, *, #6758, .F. ) ;
#5381 = ORIENTED_EDGE ( 'NONE', *, *, #6004, .F. ) ;
#5382 = CIRCLE ( 'NONE', #7322, 15.91767397667354089 ) ;
#5383 = ORIENTED_EDGE ( 'NONE', *, *, #14484, .F. ) ;
#5384 = CARTESIAN_POINT ( 'NONE',  ( 0.000000000000000000, 0.000000000000000000, 269.6944534026102360 ) ) ;
#5385 = EDGE_LOOP ( 'NONE', ( #8767, #17595, #10131, #14161 ) ) ;
#5386 = CARTESIAN_POINT ( 'NONE',  ( 25.99419088092191643, -73.82206860051539365, 248.9926560891072143 ) ) ;
#5387 = PLANE ( 'NONE',  #5701 ) ;
#5388 = CARTESIAN_POINT ( 'NONE',  ( 0.000000000000000000, 0.000000000000000000, 283.5832628385307999 ) ) ;
#5389 = VERTEX_POINT ( 'NONE', #9969 ) ;
#5390 = EDGE_CURVE ( 'NONE', #17491, #6085, #7051, .T. ) ;
#5392 = LINE ( 'NONE', #4046, #19784 ) ;
#5391 = AXIS2_PLACEMENT_3D ( 'NONE', #19017, #1818, #282 ) ;
#5393 = LINE ( 'NONE', #19314, #15663 ) ;
#5394 = EDGE_CURVE ( 'NONE', #3790, #19700, #19482, .T. ) ;
#5395 = EDGE_LOOP ( 'NONE', ( #18813, #13481, #5680, #8239, #4884 ) ) ;
#5396 = DIRECTION ( 'NONE',  ( 6.982962677686266711E-15, -0.000000000000000000, 1.000000000000000000 ) ) ;
#5397 = CARTESIAN_POINT ( 'NONE',  ( -9.381844291199351815, 57.94128254008192158, 248.9926560891072143 ) ) ;
#5398 = CARTESIAN_POINT ( 'NONE',  ( 91.98363426319514247, -42.08539992651071771, 14.88498244535480985 ) ) ;
#5399 = VECTOR ( 'NONE', #15429, 1000.000000000000000 ) ;
#5400 = DIRECTION ( 'NONE',  ( -0.000000000000000000, -0.000000000000000000, -1.000000000000000000 ) ) ;
#5401 = DIRECTION ( 'NONE',  ( 1.000000000000000000, 0.000000000000000000, 0.000000000000000000 ) ) ;
#5402 = DIRECTION ( 'NONE',  ( 0.000000000000000000, 0.000000000000000000, -1.000000000000000000 ) ) ;
#5403 = DIRECTION ( 'NONE',  ( 1.000000000000000000, 0.000000000000000000, -6.994638739193269649E-15 ) ) ;
#5404 = VERTEX_POINT ( 'NONE', #2602 ) ;
#5405 = EDGE_CURVE ( 'NONE', #7679, #14667, #5105, .T. ) ;
#5406 = DIRECTION ( 'NONE',  ( 0.000000000000000000, 0.000000000000000000, 1.000000000000000000 ) ) ;
#5407 = ORIENTED_EDGE ( 'NONE', *, *, #12722, .F. ) ;
#5408 = ORIENTED_EDGE ( 'NONE', *, *, #10832, .F. ) ;
#5409 = PLANE ( 'NONE',  #19069 ) ;
#5410 = ORIENTED_EDGE ( 'NONE', *, *, #11477, .T. ) ;
#5411 = DIRECTION ( 'NONE',  ( 1.000000000000000000, 0.000000000000000000, 0.000000000000000000 ) ) ;
#5412 = CARTESIAN_POINT ( 'NONE',  ( -0.7000608949449798057, -5.693982670708954252, 293.5832628385307999 ) ) ;
#5413 = ADVANCED_FACE ( 'NONE', ( #2495 ), #3728, .F. ) ;
#5414 = EDGE_CURVE ( 'NONE', #6230, #2720, #5749, .T. ) ;
#5415 = CARTESIAN_POINT ( 'NONE',  ( -110.0000000000000000, 285.0000000000000568, 104.9999999999999858 ) ) ;
#5416 = LINE ( 'NONE', #5223, #2143 ) ;
#5417 = VECTOR ( 'NONE', #11905, 1000.000000000000114 ) ;
#5418 = ORIENTED_EDGE ( 'NONE', *, *, #17033, .T. ) ;
#5419 = CARTESIAN_POINT ( 'NONE',  ( -126.7720928841325474, -80.18313274224119880, 49.03856716278833972 ) ) ;
#5420 = CARTESIAN_POINT ( 'NONE',  ( 97.77735676332858361, -133.5903492488113500, 7.649607847903932445 ) ) ;
#5421 = TOROIDAL_SURFACE ( 'NONE', #17510, 110.0000000000000142, 30.00000000000000000 ) ;
#5422 = ADVANCED_FACE ( 'NONE', ( #13420 ), #17499, .F. ) ;
#5423 = LINE ( 'NONE', #7056, #18656 ) ;
#5424 = CARTESIAN_POINT ( 'NONE',  ( 28.06281046684275182, -73.06915264522011455, 111.4180192758973362 ) ) ;
#5425 = ORIENTED_EDGE ( 'NONE', *, *, #12017, .F. ) ;
#5426 = CARTESIAN_POINT ( 'NONE',  ( 69.11703934647950121, -95.44259730872654757, 14.88498244535496973 ) ) ;
#5427 = CARTESIAN_POINT ( 'NONE',  ( 61.70726652483817531, 12.28122767885865407, 132.4711112102474146 ) ) ;
#5428 = DIRECTION ( 'NONE',  ( -1.000000000000000000, 0.000000000000000000, 0.000000000000000000 ) ) ;
#5429 = DIRECTION ( 'NONE',  ( 1.000000000000000000, 0.000000000000000000, 0.000000000000000000 ) ) ;
#5430 = ORIENTED_EDGE ( 'NONE', *, *, #3856, .T. ) ;
#5431 = B_SPLINE_CURVE_WITH_KNOTS ( 'NONE', 3,
 ( #16190, #1762, #536, #17431, #11270, #2179, #3406, #8301, #19067, #17724, #9733, #19157, #5151, #12804, #7997, #13001, #14243, #222, #14547, #12903, #3701, #6479, #12701, #18964, #11376, #14447, #16087, #3603, #5051, #8095, #6583, #9637, #326, #15887 ),
 .UNSPECIFIED., .F., .F.,
 ( 4, 2, 2, 2, 2, 2, 2, 2, 2, 2, 2, 2, 2, 2, 2, 2, 4 ),
 ( 0.08723304891271140005, 0.09476463103839000146, 0.1022962131640685890, 0.1060620042269078966, 0.1098277952897471904, 0.1173593774154258196, 0.1324225416667830502, 0.1399541237924616655, 0.1437199148553010009, 0.1474857059181403085, 0.1625488701694974836, 0.1776120344208546864, 0.1851436165465332739, 0.1926751986722118892, 0.2002067807978905045, 0.2039725718607297567, 0.2077383629235690921 ),
 .UNSPECIFIED. ) ;
#5432 = DIRECTION ( 'NONE',  ( -0.9749279121818257288, 0.2225209339563050392, -0.000000000000000000 ) ) ;
#5433 = CARTESIAN_POINT ( 'NONE',  ( -1.379293853801755176, 78.26059000578311498, 112.7772637782949943 ) ) ;
#5434 = ORIENTED_EDGE ( 'NONE', *, *, #18110, .F. ) ;
#5435 = AXIS2_PLACEMENT_3D ( 'NONE', #10351, #1254, #10657 ) ;
#5436 = ORIENTED_EDGE ( 'NONE', *, *, #3283, .F. ) ;
#5437 = EDGE_LOOP ( 'NONE', ( #4145, #3543, #16654, #16540 ) ) ;
#5438 = DIRECTION ( 'NONE',  ( 0.1736481776669273336, 0.9848077530122085754, 0.000000000000000000 ) ) ;
#5439 = ORIENTED_EDGE ( 'NONE', *, *, #656, .F. ) ;
#5440 = CARTESIAN_POINT ( 'NONE',  ( 99.73767742489731347, -112.0463336856532521, -10.00000000004823519 ) ) ;
#5441 = CARTESIAN_POINT ( 'NONE',  ( -95.50801338651713479, -116.1654322105520265, 8.498518821464802642 ) ) ;
#5442 = ORIENTED_EDGE ( 'NONE', *, *, #2615, .F. ) ;
#5443 = VECTOR ( 'NONE', #7750, 1000.000000000000114 ) ;
#5444 = DIRECTION ( 'NONE',  ( -0.1736481776669268895, 0.9848077530122086864, 2.152196535136390479E-15 ) ) ;
#5445 = DIRECTION ( 'NONE',  ( 0.1736481776669374366, -0.9848077530122067991, 0.000000000000000000 ) ) ;
#5446 = DIRECTION ( 'NONE',  ( -0.000000000000000000, -0.000000000000000000, -1.000000000000000000 ) ) ;
#5447 = DIRECTION ( 'NONE',  ( -0.7660444431189792347, 0.6427876096865379196, 0.000000000000000000 ) ) ;
#5448 = CARTESIAN_POINT ( 'NONE',  ( 176.1792632384392334, -186.5724904703758682, 40.00000000000000000 ) ) ;
#5449 = DIRECTION ( 'NONE',  ( 0.000000000000000000, 1.000000000000000000, 0.000000000000000000 ) ) ;
#5450 = ORIENTED_EDGE ( 'NONE', *, *, #13991, .T. ) ;
#5451 = VECTOR ( 'NONE', #882, 1000.000000000000000 ) ;
#5452 = CARTESIAN_POINT ( 'NONE',  ( 126.5370453525553671, 80.55045718954892209, 49.99999999999999289 ) ) ;
#5453 = DIRECTION ( 'NONE',  ( -0.9394263059140725014, 0.3427509529624092055, 0.000000000000000000 ) ) ;
#5454 = EDGE_LOOP ( 'NONE', ( #8913, #11367, #7685, #5550 ) ) ;
#5455 = CIRCLE ( 'NONE', #15240, 60.74260934110282051 ) ;
#5456 = ORIENTED_EDGE ( 'NONE', *, *, #19496, .T. ) ;
#5457 = VERTEX_POINT ( 'NONE', #19977 ) ;
#5458 = DIRECTION ( 'NONE',  ( -0.3420201433256725987, 0.9396926207859068736, 0.000000000000000000 ) ) ;
#5459 = AXIS2_PLACEMENT_3D ( 'NONE', #5952, #4302, #16789 ) ;
#5460 = DIRECTION ( 'NONE',  ( 0.3420201433256790380, -0.9396926207859046531, 0.000000000000000000 ) ) ;
#5461 = DIRECTION ( 'NONE',  ( -0.6692498792541777819, -0.7430374143461878633, 0.000000000000000000 ) ) ;
#5462 = DIRECTION ( 'NONE',  ( -0.9749279121818257288, 0.2225209339563050392, -0.000000000000000000 ) ) ;
#5463 = CARTESIAN_POINT ( 'NONE',  ( -23.23469325536272478, -13.41455640552162443, 14.88498244535561454 ) ) ;
#5464 = ADVANCED_FACE ( 'NONE', ( #7497 ), #12196, .F. ) ;
#5465 = CARTESIAN_POINT ( 'NONE',  ( -51.24071425735603924, 32.61983739937744531, 283.5832628385307999 ) ) ;
#5466 = CARTESIAN_POINT ( 'NONE',  ( -123.6158562626643516, -84.97727779989590147, -9.999999999476957058 ) ) ;
#5467 = CARTESIAN_POINT ( 'NONE',  ( 132.7096788433826191, -70.03826381905518872, 5.661456724840400412 ) ) ;
#5468 = CARTESIAN_POINT ( 'NONE',  ( 135.1060089022256534, -65.16414933467420667, 49.99999999999999289 ) ) ;
#5469 = DIRECTION ( 'NONE',  ( 0.5000000000000101030, -0.8660254037844328234, 0.000000000000000000 ) ) ;
#5470 = ORIENTED_EDGE ( 'NONE', *, *, #10225, .T. ) ;
#5471 = VECTOR ( 'NONE', #16136, 1000.000000000000227 ) ;
#5472 = SHAPE_REPRESENTATION ( 'Vane Disc', ( #18639 ), #4580 ) ;
#5474 = ORIENTED_EDGE ( 'NONE', *, *, #17363, .T. ) ;
#5473 = CIRCLE ( 'NONE', #15924, 106.4288957539801146 ) ;
#5475 = ADVANCED_FACE ( 'NONE', ( #17122 ), #9658, .F. ) ;
#5476 = AXIS2_PLACEMENT_3D ( 'NONE', #359, #9672, #11412 ) ;
#5477 = ORIENTED_EDGE ( 'NONE', *, *, #11374, .T. ) ;
#5478 = VERTEX_POINT ( 'NONE', #15375 ) ;
#5479 = ADVANCED_FACE ( 'NONE', ( #1364 ), #7593, .T. ) ;
#5480 = DIRECTION ( 'NONE',  ( 0.9848077530122103518, -0.1736481776669172583, 0.000000000000000000 ) ) ;
#5481 = EDGE_LOOP ( 'NONE', ( #11039, #18396, #16367, #10534 ) ) ;
#5482 = CARTESIAN_POINT ( 'NONE',  ( 0.000000000000000000, 0.000000000000000000, 293.5832628385307999 ) ) ;
#5483 = FACE_OUTER_BOUND ( 'NONE', #472, .T. ) ;
#5484 = CARTESIAN_POINT ( 'NONE',  ( 0.000000000000000000, 0.000000000000000000, 293.5832628385307999 ) ) ;
#5485 = ORIENTED_EDGE ( 'NONE', *, *, #16912, .F. ) ;
#5486 = LINE ( 'NONE', #10092, #5417 ) ;
#5487 = DIRECTION ( 'NONE',  ( -0.000000000000000000, -0.000000000000000000, 1.000000000000000000 ) ) ;
#5488 = CIRCLE ( 'NONE', #16925, 7.500000000000006217 ) ;
#5489 = ADVANCED_FACE ( 'NONE', ( #18666 ), #9341, .T. ) ;
#5490 = ORIENTED_EDGE ( 'NONE', *, *, #6871, .T. ) ;
#5491 = LINE ( 'NONE', #3948, #17945 ) ;
#5492 = VECTOR ( 'NONE', #3813, 1000.000000000000000 ) ;
#5493 = DIRECTION ( 'NONE',  ( 0.6692498792541753394, 0.7430374143461900838, 0.000000000000000000 ) ) ;
#5494 = CARTESIAN_POINT ( 'NONE',  ( -62.91215678473957240, 0.8220851292433130064, 293.5832628385307999 ) ) ;
#5495 = FACE_OUTER_BOUND ( 'NONE', #8432, .T. ) ;
#5496 = CARTESIAN_POINT ( 'NONE',  ( -110.0000000000000000, 285.0000000000000568, 104.9999999999999858 ) ) ;
#5497 = DIRECTION ( 'NONE',  ( 0.4999999999999925060, -0.8660254037844429265, -3.228294802704592424E-15 ) ) ;
#5498 = EDGE_LOOP ( 'NONE', ( #4980, #14689, #7232, #6679 ) ) ;
#5499 = ADVANCED_FACE ( 'NONE', ( #1572, #7807, #19774, #3613, #8103, #11073 ), #10971, .F. ) ;
#5500 = LINE ( 'NONE', #12965, #14815 ) ;
#5501 = AXIS2_PLACEMENT_3D ( 'NONE', #11240, #9706, #12971 ) ;
#5502 = ORIENTED_EDGE ( 'NONE', *, *, #6159, .T. ) ;
#5503 = ADVANCED_FACE ( 'NONE', ( #1872 ), #14148, .F. ) ;
#5504 = VECTOR ( 'NONE', #8430, 1000.000000000000000 ) ;
#5505 = EDGE_LOOP ( 'NONE', ( #18357, #12771, #3377, #681, #669 ) ) ;
#5506 = ADVANCED_FACE ( 'NONE', ( #441 ), #4853, .T. ) ;
#5507 = CARTESIAN_POINT ( 'NONE',  ( 0.000000000000000000, 0.000000000000000000, -105.0000000000000142 ) ) ;
#5508 = AXIS2_PLACEMENT_3D ( 'NONE', #7885, #1963, #9428 ) ;
#5509 = EDGE_LOOP ( 'NONE', ( #4060, #17213 ) ) ;
#5510 = CARTESIAN_POINT ( 'NONE',  ( -134.7652707650784407, -31.41120252075685215, -19.73219286542039441 ) ) ;
#5511 = CARTESIAN_POINT ( 'NONE',  ( 0.000000000000000000, 0.000000000000000000, 293.5832628385307999 ) ) ;
#5512 = DIRECTION ( 'NONE',  ( -1.000000000000000000, 0.000000000000000000, -0.000000000000000000 ) ) ;
#5513 = CARTESIAN_POINT ( 'NONE',  ( -47.29944656917786006, -41.48948842197101783, 293.5832628385307999 ) ) ;
#5514 = ORIENTED_EDGE ( 'NONE', *, *, #1426, .T. ) ;
#5515 = EDGE_CURVE ( 'NONE', #1786, #19610, #1982, .T. ) ;
#5516 = CARTESIAN_POINT ( 'NONE',  ( -133.1207282269168388, -69.13111487717780790, 41.23326533417627360 ) ) ;
#5517 = CARTESIAN_POINT ( 'NONE',  ( -31.77187437101503775, -51.77076963420834943, 293.5832628385307999 ) ) ;
#5518 = VECTOR ( 'NONE', #17904, 1000.000000000000227 ) ;
#5519 = DIRECTION ( 'NONE',  ( 0.000000000000000000, 0.000000000000000000, 1.000000000000000000 ) ) ;
#5520 = CARTESIAN_POINT ( 'NONE',  ( 28.94983032429829350, -53.40245231972188833, 293.5832628385307999 ) ) ;
#5521 = VECTOR ( 'NONE', #1896, 1000.000000000000000 ) ;
#5522 = ORIENTED_EDGE ( 'NONE', *, *, #13615, .T. ) ;
#5523 = DIRECTION ( 'NONE',  ( 0.000000000000000000, 1.000000000000000000, 0.000000000000000000 ) ) ;
#5524 = CARTESIAN_POINT ( 'NONE',  ( 85.34080972464066406, -123.3578596465555677, -1.367079200094239333 ) ) ;
#5525 = LINE ( 'NONE', #13179, #6632 ) ;
#5526 = VERTEX_POINT ( 'NONE', #15792 ) ;
#5527 = DIRECTION ( 'NONE',  ( 1.000000000000000000, 0.000000000000000000, 0.000000000000000000 ) ) ;
#5528 = DIRECTION ( 'NONE',  ( 6.982962677686266711E-15, -0.000000000000000000, 1.000000000000000000 ) ) ;
#5529 = EDGE_CURVE ( 'NONE', #5526, #4551, #11607, .T. ) ;
#5530 = VERTEX_POINT ( 'NONE', #970 ) ;
#5531 = ADVANCED_FACE ( 'NONE', ( #5296 ), #18069, .T. ) ;
#5532 = EDGE_CURVE ( 'NONE', #16978, #16737, #12264, .T. ) ;
#5533 = ORIENTED_EDGE ( 'NONE', *, *, #12630, .F. ) ;
#5534 = EDGE_CURVE ( 'NONE', #13478, #2029, #13052, .T. ) ;
#5535 = AXIS2_PLACEMENT_3D ( 'NONE', #464, #9971, #14680 ) ;
#5536 = VECTOR ( 'NONE', #17874, 1000.000000000000000 ) ;
#5537 = CARTESIAN_POINT ( 'NONE',  ( 73.82206860051529418, 25.99419088092216867, 248.9926560891072143 ) ) ;
#5538 = DIRECTION ( 'NONE',  ( 0.9396926207859082059, 0.3420201433256694901, 0.000000000000000000 ) ) ;
#5539 = ORIENTED_EDGE ( 'NONE', *, *, #13761, .F. ) ;
#5540 = CARTESIAN_POINT ( 'NONE',  ( 101.9549241234500983, -127.6987521375408079, 1.655170884984768165 ) ) ;
#5541 = CARTESIAN_POINT ( 'NONE',  ( -93.45568245712546229, -117.3306176392020888, -8.420502908542239595 ) ) ;
#5542 = CARTESIAN_POINT ( 'NONE',  ( -84.30790708731534266, -124.0658650269852501, 0.4226591875635389295 ) ) ;
#5543 = FACE_OUTER_BOUND ( 'NONE', #8293, .T. ) ;
#5544 = CARTESIAN_POINT ( 'NONE',  ( -40.32479851956769323, 67.08601213326579682, 132.4711112102474146 ) ) ;
#5545 = DIRECTION ( 'NONE',  ( -0.000000000000000000, -0.000000000000000000, -1.000000000000000000 ) ) ;
#5546 = CARTESIAN_POINT ( 'NONE',  ( -60.00000000000000000, -2.094888803305880013E-13, -105.0000000000000142 ) ) ;
#5547 = VECTOR ( 'NONE', #11347, 1000.000000000000114 ) ;
#5548 = DIRECTION ( 'NONE',  ( 6.982962677686266711E-15, -0.000000000000000000, 1.000000000000000000 ) ) ;
#5549 = CIRCLE ( 'NONE', #2937, 99.99999999999997158 ) ;
#5550 = ORIENTED_EDGE ( 'NONE', *, *, #1860, .T. ) ;
#5551 = DIRECTION ( 'NONE',  ( -1.000000000000000000, 0.000000000000000000, 0.000000000000000000 ) ) ;
#5552 = CARTESIAN_POINT ( 'NONE',  ( 53.40063514825077107, 28.94886449118924432, 293.5832628385307999 ) ) ;
#5553 = EDGE_CURVE ( 'NONE', #3260, #5786, #5392, .T. ) ;
#5554 = ORIENTED_EDGE ( 'NONE', *, *, #2992, .F. ) ;
#5555 = VERTEX_POINT ( 'NONE', #7025 ) ;
#5556 = EDGE_CURVE ( 'NONE', #17774, #17628, #19313, .T. ) ;
#5557 = CARTESIAN_POINT ( 'NONE',  ( -156.4179374840092862, -52.02840013024096066, 60.00000000000000000 ) ) ;
#5558 = ORIENTED_EDGE ( 'NONE', *, *, #18687, .F. ) ;
#5559 = AXIS2_PLACEMENT_3D ( 'NONE', #6976, #543, #4095 ) ;
#5560 = CARTESIAN_POINT ( 'NONE',  ( 134.6687524777004228, -73.33058021821595673, 8.085668793728526538 ) ) ;
#5561 = CARTESIAN_POINT ( 'NONE',  ( -131.9010376021428783, -71.43117396976207090, -3.793297712624513540 ) ) ;
#5562 = DIRECTION ( 'NONE',  ( 0.000000000000000000, 0.000000000000000000, 1.000000000000000000 ) ) ;
#5563 = DIRECTION ( 'NONE',  ( -0.000000000000000000, -0.000000000000000000, 1.000000000000000000 ) ) ;
#5564 = FACE_OUTER_BOUND ( 'NONE', #10194, .T. ) ;
#5565 = ORIENTED_EDGE ( 'NONE', *, *, #11939, .F. ) ;
#5566 = LINE ( 'NONE', #11885, #13034 ) ;
#5567 = CARTESIAN_POINT ( 'NONE',  ( -128.7737027234273626, -76.92703321535461214, -7.688188765993792195 ) ) ;
#5568 = CARTESIAN_POINT ( 'NONE',  ( 134.1858200530627983, -67.03963421358798769, 2.112429552066504179 ) ) ;
#5569 = FACE_OUTER_BOUND ( 'NONE', #12440, .T. ) ;
#5570 = DIRECTION ( 'NONE',  ( 0.000000000000000000, 0.000000000000000000, -1.000000000000000000 ) ) ;
#5571 = LINE ( 'NONE', #2134, #15512 ) ;
#5572 = VERTEX_POINT ( 'NONE', #8552 ) ;
#5573 = AXIS2_PLACEMENT_3D ( 'NONE', #19141, #7774, #411 ) ;
#5574 = ORIENTED_EDGE ( 'NONE', *, *, #508, .F. ) ;
#5575 = ORIENTED_EDGE ( 'NONE', *, *, #2391, .T. ) ;
#5576 = EDGE_LOOP ( 'NONE', ( #7626, #17569, #4274, #4395 ) ) ;
#5577 = EDGE_CURVE ( 'NONE', #18899, #15118, #5486, .T. ) ;
#5578 = VERTEX_POINT ( 'NONE', #11803 ) ;
#5579 = VECTOR ( 'NONE', #7724, 1000.000000000000227 ) ;
#5580 = CARTESIAN_POINT ( 'NONE',  ( 78.68887634719571622, -147.8252249328912740, 49.99999999999999289 ) ) ;
#5581 = FACE_OUTER_BOUND ( 'NONE', #14740, .T. ) ;
#5582 = ORIENTED_EDGE ( 'NONE', *, *, #15905, .T. ) ;
#5583 = AXIS2_PLACEMENT_3D ( 'NONE', #11790, #13322, #17852 ) ;
#5584 = FACE_OUTER_BOUND ( 'NONE', #6798, .T. ) ;
#5585 = DIRECTION ( 'NONE',  ( 1.000000000000000000, 0.000000000000000000, 0.000000000000000000 ) ) ;
#5586 = VERTEX_POINT ( 'NONE', #3845 ) ;
#5587 = CARTESIAN_POINT ( 'NONE',  ( 0.2993243175132189737, -5.729042578294415655, 293.5832628385307999 ) ) ;
#5588 = ADVANCED_FACE ( 'NONE', ( #5584 ), #10282, .F. ) ;
#5589 = DIRECTION ( 'NONE',  ( 0.000000000000000000, 0.000000000000000000, -1.000000000000000000 ) ) ;
#5590 = FACE_OUTER_BOUND ( 'NONE', #5576, .T. ) ;
#5591 = CARTESIAN_POINT ( 'NONE',  ( 48.09719419928496364, 107.5784105627835174, 14.88498244535511539 ) ) ;
#5592 = AXIS2_PLACEMENT_3D ( 'NONE', #3618, #4856, #9648 ) ;
#5593 = CARTESIAN_POINT ( 'NONE',  ( 128.2779226595531270, 102.2982297021113141, 60.00000000000000000 ) ) ;
#5594 = FACE_OUTER_BOUND ( 'NONE', #3425, .T. ) ;
#5595 = VERTEX_POINT ( 'NONE', #8652 ) ;
#5596 = AXIS2_PLACEMENT_3D ( 'NONE', #828, #2472, #8704 ) ;
#5597 = DIRECTION ( 'NONE',  ( 0.000000000000000000, 0.000000000000000000, 1.000000000000000000 ) ) ;
#5598 = EDGE_LOOP ( 'NONE', ( #10439, #14759 ) ) ;
#5599 = AXIS2_PLACEMENT_3D ( 'NONE', #7992, #218, #1351 ) ;
#5600 = ORIENTED_EDGE ( 'NONE', *, *, #1484, .F. ) ;
#5601 = EDGE_CURVE ( 'NONE', #16315, #15959, #17976, .T. ) ;
#5602 = CARTESIAN_POINT ( 'NONE',  ( 62.95000000000000284, 0.000000000000000000, 0.000000000000000000 ) ) ;
#5603 = EDGE_CURVE ( 'NONE', #295, #6917, #13231, .T. ) ;
#5604 = ORIENTED_EDGE ( 'NONE', *, *, #15675, .T. ) ;
#5605 = ORIENTED_EDGE ( 'NONE', *, *, #7734, .F. ) ;
#5606 = CARTESIAN_POINT ( 'NONE',  ( 28.43859219408686911, 46.49849886828724976, 248.9926560891072143 ) ) ;
#5607 = CARTESIAN_POINT ( 'NONE',  ( 36.99514631729018532, -48.17959877923561862, 293.5832628385307999 ) ) ;
#5608 = CARTESIAN_POINT ( 'NONE',  ( 0.000000000000000000, 0.000000000000000000, 283.5832628385307999 ) ) ;
#5609 = CARTESIAN_POINT ( 'NONE',  ( 0.000000000000000000, 0.000000000000000000, 132.4711112102474146 ) ) ;
#5610 = ORIENTED_EDGE ( 'NONE', *, *, #838, .F. ) ;
#5611 = EDGE_CURVE ( 'NONE', #3122, #10094, #14793, .T. ) ;
#5612 = DIRECTION ( 'NONE',  ( -0.6718749999999997780, -0.7406645559057084549, 0.000000000000000000 ) ) ;
#5613 = DIRECTION ( 'NONE',  ( 1.000000000000000000, 0.000000000000000000, -0.000000000000000000 ) ) ;
#5614 = EDGE_CURVE ( 'NONE', #9195, #16956, #580, .T. ) ;
#5615 = CARTESIAN_POINT ( 'NONE',  ( 60.72279549541555355, -1.629937663769388090, 293.5832628385307999 ) ) ;
#5616 = EDGE_CURVE ( 'NONE', #8743, #19246, #10185, .T. ) ;
#5617 = DIRECTION ( 'NONE',  ( 0.000000000000000000, 0.000000000000000000, 1.000000000000000000 ) ) ;
#5618 = ORIENTED_EDGE ( 'NONE', *, *, #17150, .T. ) ;
#5619 = CIRCLE ( 'NONE', #19029, 112.8770930172170210 ) ;
#5620 = PLANE ( 'NONE',  #14914 ) ;
#5621 = DIRECTION ( 'NONE',  ( -0.000000000000000000, -0.000000000000000000, 1.000000000000000000 ) ) ;
#5622 = CARTESIAN_POINT ( 'NONE',  ( 58.69016442926520938, 1.379293853802370018, 112.7772637782949516 ) ) ;
#5623 = VERTEX_POINT ( 'NONE', #7123 ) ;
#5624 = CARTESIAN_POINT ( 'NONE',  ( -45.46712722958807973, 40.27908801170008957, 293.5832628385307999 ) ) ;
#5625 = DIRECTION ( 'NONE',  ( -0.000000000000000000, -0.000000000000000000, -1.000000000000000000 ) ) ;
#5626 = ORIENTED_EDGE ( 'NONE', *, *, #9175, .F. ) ;
#5627 = EDGE_LOOP ( 'NONE', ( #1726, #3042, #13561, #18515 ) ) ;
#5628 = EDGE_CURVE ( 'NONE', #13590, #15181, #683, .T. ) ;
#5629 = ADVANCED_FACE ( 'NONE', ( #19408 ), #19692, .T. ) ;
#5630 = ORIENTED_EDGE ( 'NONE', *, *, #14367, .T. ) ;
#5631 = CARTESIAN_POINT ( 'NONE',  ( 14.94814811854963388, -76.83212392882498420, 112.0427633081291816 ) ) ;
#5632 = DIRECTION ( 'NONE',  ( 0.3088643371590157338, -0.9511061040868794558, 0.000000000000000000 ) ) ;
#5633 = CIRCLE ( 'NONE', #13134, 60.74260934110282051 ) ;
#5634 = VERTEX_POINT ( 'NONE', #5689 ) ;
#5635 = CIRCLE ( 'NONE', #13805, 65.74260934110282051 ) ;
#5636 = CARTESIAN_POINT ( 'NONE',  ( 100.0290433904799698, -111.7820284656621368, 0.3810183304975476859 ) ) ;
#5637 = FACE_OUTER_BOUND ( 'NONE', #18493, .T. ) ;
#5638 = EDGE_CURVE ( 'NONE', #3301, #10259, #9069, .T. ) ;
#5639 = AXIS2_PLACEMENT_3D ( 'NONE', #7350, #10218, #19445 ) ;
#5640 = EDGE_CURVE ( 'NONE', #18497, #5054, #2620, .T. ) ;
#5641 = CARTESIAN_POINT ( 'NONE',  ( -134.7188131032333445, -72.93593548660989256, 1.387778780781445676E-14 ) ) ;
#5642 = CARTESIAN_POINT ( 'NONE',  ( 32.50000000000000000, 3.980102097228898626E-15, -110.0000000000000000 ) ) ;
#5643 = CARTESIAN_POINT ( 'NONE',  ( -7.948651060879014629, 60.22029172860440838, 283.5832628385307999 ) ) ;
#5644 = DIRECTION ( 'NONE',  ( -0.000000000000000000, -0.000000000000000000, 1.000000000000000000 ) ) ;
#5645 = CARTESIAN_POINT ( 'NONE',  ( 0.000000000000000000, 0.000000000000000000, 60.00000000000000000 ) ) ;
#5646 = CARTESIAN_POINT ( 'NONE',  ( 1.379293853801755176, -62.90240729679781850, 132.4711112102474146 ) ) ;
#5647 = ORIENTED_EDGE ( 'NONE', *, *, #9199, .T. ) ;
#5648 = DIRECTION ( 'NONE',  ( 6.982962677686266711E-15, -0.000000000000000000, 1.000000000000000000 ) ) ;
#5649 = DIRECTION ( 'NONE',  ( 0.000000000000000000, 0.000000000000000000, 1.000000000000000000 ) ) ;
#5650 = AXIS2_PLACEMENT_3D ( 'NONE', #18746, #15355, #13610 ) ;
#5651 = AXIS2_PLACEMENT_3D ( 'NONE', #13273, #3884, #13081 ) ;
#5652 = ORIENTED_EDGE ( 'NONE', *, *, #3994, .T. ) ;
#5653 = EDGE_LOOP ( 'NONE', ( #193, #4758, #14383, #11897 ) ) ;
#5654 = EDGE_CURVE ( 'NONE', #13855, #18133, #15565, .T. ) ;
#5655 =( NAMED_UNIT ( * ) PLANE_ANGLE_UNIT ( ) SI_UNIT ( $, .RADIAN. ) );
#5656 = CONICAL_SURFACE ( 'NONE', #16440, 9.000000000000000000, 1.047197551196600296 ) ;
#5657 = VERTEX_POINT ( 'NONE', #13544 ) ;
#5658 = CARTESIAN_POINT ( 'NONE',  ( 0.000000000000000000, 0.000000000000000000, -105.0000000000000142 ) ) ;
#5659 = AXIS2_PLACEMENT_3D ( 'NONE', #13905, #20150, #12367 ) ;
#5660 = VERTEX_POINT ( 'NONE', #1284 ) ;
#5661 = DIRECTION ( 'NONE',  ( -0.000000000000000000, -0.000000000000000000, -1.000000000000000000 ) ) ;
#5662 = FACE_OUTER_BOUND ( 'NONE', #13250, .T. ) ;
#5663 = AXIS2_PLACEMENT_3D ( 'NONE', #17493, #17393, #11341 ) ;
#5664 = CARTESIAN_POINT ( 'NONE',  ( 7.350000000000000533, 5.196152422706627583, 9.000000000000001776 ) ) ;
#5665 = EDGE_CURVE ( 'NONE', #8743, #7392, #15212, .T. ) ;
#5666 = EDGE_CURVE ( 'NONE', #15773, #11866, #12518, .T. ) ;
#5667 = CARTESIAN_POINT ( 'NONE',  ( -60.22029172860436574, -7.948651060879222463, 283.5832628385307999 ) ) ;
#5668 = ORIENTED_EDGE ( 'NONE', *, *, #13265, .F. ) ;
#5669 = CARTESIAN_POINT ( 'NONE',  ( -133.2435246741110006, -68.89240257401093004, 40.00000000000000000 ) ) ;
#5670 = DIRECTION ( 'NONE',  ( -0.9009688679024212554, 0.4338837391175534575, 0.000000000000000000 ) ) ;
#5671 = CARTESIAN_POINT ( 'NONE',  ( 134.7188131032333445, -72.93593548660993520, 10.00000000000000533 ) ) ;
#5672 = VECTOR ( 'NONE', #13827, 1000.000000000000000 ) ;
#5673 = CARTESIAN_POINT ( 'NONE',  ( 0.000000000000000000, 0.000000000000000000, 283.5832628385307999 ) ) ;
#5674 = PLANE ( 'NONE',  #6145 ) ;
#5675 = EDGE_CURVE ( 'NONE', #4234, #2109, #20125, .T. ) ;
#5676 = ORIENTED_EDGE ( 'NONE', *, *, #10721, .T. ) ;
#5677 = AXIS2_PLACEMENT_3D ( 'NONE', #5920, #15421, #9284 ) ;
#5678 = APPLICATION_CONTEXT ( 'automotive_design' ) ;
#5679 = VERTEX_POINT ( 'NONE', #18369 ) ;
#5680 = ORIENTED_EDGE ( 'NONE', *, *, #4603, .F. ) ;
#5681 = EDGE_LOOP ( 'NONE', ( #5425, #11818, #5065, #4733 ) ) ;
#5682 = ORIENTED_EDGE ( 'NONE', *, *, #11479, .F. ) ;
#5683 = VECTOR ( 'NONE', #8609, 1000.000000000000000 ) ;
#5684 = CARTESIAN_POINT ( 'NONE',  ( 62.95000000000000284, 0.000000000000000000, 0.000000000000000000 ) ) ;
#5685 = DIRECTION ( 'NONE',  ( -0.000000000000000000, -1.000000000000000000, -0.000000000000000000 ) ) ;
#5686 = VECTOR ( 'NONE', #13049, 1000.000000000000000 ) ;
#5687 = DIRECTION ( 'NONE',  ( 0.000000000000000000, 0.000000000000000000, 1.000000000000000000 ) ) ;
#5688 = ORIENTED_EDGE ( 'NONE', *, *, #9651, .F. ) ;
#5689 = CARTESIAN_POINT ( 'NONE',  ( -78.68887634719366986, -147.8252249328922687, 49.99999999999999289 ) ) ;
#5690 = DIRECTION ( 'NONE',  ( 0.000000000000000000, 0.000000000000000000, -1.000000000000000000 ) ) ;
#5691 = ORIENTED_EDGE ( 'NONE', *, *, #16771, .F. ) ;
#5692 = DIRECTION ( 'NONE',  ( 1.000000000000000000, 0.000000000000000000, 0.000000000000000000 ) ) ;
#5693 = CARTESIAN_POINT ( 'NONE',  ( 44.43084819159276577, -38.35506425062471436, 248.9926560891072143 ) ) ;
#5694 = CARTESIAN_POINT ( 'NONE',  ( -131.2500704209022615, -90.93860529234680712, 6.324512672832136480E-16 ) ) ;
#5695 = DIRECTION ( 'NONE',  ( 1.000000000000000000, 0.000000000000000000, -0.000000000000000000 ) ) ;
#5696 = CARTESIAN_POINT ( 'NONE',  ( 132.6415777375408425, -85.19230204981589338, 39.23511747715267717 ) ) ;
#5697 = CIRCLE ( 'NONE', #18795, 7.500000000000007994 ) ;
#5698 = DIRECTION ( 'NONE',  ( -6.982962677686266711E-15, 0.000000000000000000, -1.000000000000000000 ) ) ;
#5699 = ORIENTED_EDGE ( 'NONE', *, *, #16613, .F. ) ;
#5700 = PLANE ( 'NONE',  #11296 ) ;
#5701 = AXIS2_PLACEMENT_3D ( 'NONE', #16237, #9884, #8348 ) ;
#5702 = ORIENTED_EDGE ( 'NONE', *, *, #3358, .F. ) ;
#5703 = VERTEX_POINT ( 'NONE', #19994 ) ;
#5704 = CARTESIAN_POINT ( 'NONE',  ( 0.000000000000000000, 0.000000000000000000, 0.000000000000000000 ) ) ;
#5705 = VERTEX_POINT ( 'NONE', #1383 ) ;
#5706 = VERTEX_POINT ( 'NONE', #13649 ) ;
#5707 = AXIS2_PLACEMENT_3D ( 'NONE', #9737, #11275, #12497 ) ;
#5708 = DIRECTION ( 'NONE',  ( 0.000000000000000000, 0.000000000000000000, 1.000000000000000000 ) ) ;
#5709 = CARTESIAN_POINT ( 'NONE',  ( -82.39904996721718078, -125.3411509769706242, 33.95830863599796601 ) ) ;
#5710 = LINE ( 'NONE', #18188, #5368 ) ;
#5711 = VECTOR ( 'NONE', #7159, 1000.000000000000227 ) ;
#5712 = LINE ( 'NONE', #16659, #7055 ) ;
#5713 = DIRECTION ( 'NONE',  ( -0.000000000000000000, -0.000000000000000000, 1.000000000000000000 ) ) ;
#5714 = VERTEX_POINT ( 'NONE', #13856 ) ;
#5715 = CARTESIAN_POINT ( 'NONE',  ( 0.000000000000000000, 0.000000000000000000, 293.5832628385307999 ) ) ;
#5716 = DIRECTION ( 'NONE',  ( -1.000000000000000000, 0.000000000000000000, 0.000000000000000000 ) ) ;
#5717 = ADVANCED_FACE ( 'NONE', ( #9046 ), #7715, .T. ) ;
#5718 = CARTESIAN_POINT ( 'NONE',  ( 110.0000000000000142, 0.000000000000000000, -9.999999999999994671 ) ) ;
#5719 = DIRECTION ( 'NONE',  ( -1.000000000000000000, 0.000000000000000000, 0.000000000000000000 ) ) ;
#5720 = EDGE_LOOP ( 'NONE', ( #12365, #11062, #3445, #18934 ) ) ;
#5721 = DIRECTION ( 'NONE',  ( 0.000000000000000000, 0.000000000000000000, 1.000000000000000000 ) ) ;
#5722 = CARTESIAN_POINT ( 'NONE',  ( -133.8357118474723961, -78.97256401901071854, 37.04716089610885632 ) ) ;
#5723 = CIRCLE ( 'NONE', #4077, 79.75827554147308263 ) ;
#5724 = DIRECTION ( 'NONE',  ( -6.982962677686266711E-15, 0.000000000000000000, -1.000000000000000000 ) ) ;
#5725 = EDGE_LOOP ( 'NONE', ( #2767, #10803 ) ) ;
#5726 = FACE_OUTER_BOUND ( 'NONE', #7632, .T. ) ;
#5727 = CYLINDRICAL_SURFACE ( 'NONE', #18402, 3.224098631618460331 ) ;
#5728 = ORIENTED_EDGE ( 'NONE', *, *, #14857, .F. ) ;
#5729 = ADVANCED_FACE ( 'NONE', ( #16728 ), #15290, .F. ) ;
#5730 = VERTEX_POINT ( 'NONE', #15188 ) ;
#5731 = CYLINDRICAL_SURFACE ( 'NONE', #14969, 15.91767397667354800 ) ;
#5732 = ADVANCED_FACE ( 'NONE', ( #8944 ), #4558, .T. ) ;
#5733 = EDGE_CURVE ( 'NONE', #14920, #8471, #2924, .T. ) ;
#5734 = VERTEX_POINT ( 'NONE', #19897 ) ;
#5735 = EDGE_CURVE ( 'NONE', #11666, #14612, #14583, .T. ) ;
#5736 = DIRECTION ( 'NONE',  ( -0.8830229359480271656, -0.4693298356057563625, 0.000000000000000000 ) ) ;
#5737 = CARTESIAN_POINT ( 'NONE',  ( 59.30716253403183913, -13.12726406102058441, 283.5832628385307999 ) ) ;
#5738 = ORIENTED_EDGE ( 'NONE', *, *, #960, .T. ) ;
#5739 = AXIS2_PLACEMENT_3D ( 'NONE', #9735, #4952, #538 ) ;
#5740 = CARTESIAN_POINT ( 'NONE',  ( 99.33980890135488551, -112.3956798702031676, 0.8361447343429230239 ) ) ;
#5741 = CARTESIAN_POINT ( 'NONE',  ( -100.0291087224201334, -111.7819692016497015, 0.3809852373215633636 ) ) ;
#5742 = EDGE_CURVE ( 'NONE', #19269, #2533, #10638, .T. ) ;
#5743 = DIRECTION ( 'NONE',  ( 0.000000000000000000, 0.000000000000000000, 1.000000000000000000 ) ) ;
#5744 = CARTESIAN_POINT ( 'NONE',  ( 0.8220851292435327196, 58.69016442926522359, 112.7772637782949943 ) ) ;
#5745 = PLANE ( 'NONE',  #12819 ) ;
#5746 = DIRECTION ( 'NONE',  ( -0.9781142164131910732, 0.2080686897406944236, 0.000000000000000000 ) ) ;
#5747 = CARTESIAN_POINT ( 'NONE',  ( -68.18670162478832708, -38.41834839689356329, 110.9660488491356887 ) ) ;
#5748 = DIRECTION ( 'NONE',  ( 1.000000000000000000, 0.000000000000000000, -0.000000000000000000 ) ) ;
#5749 = CIRCLE ( 'NONE', #16211, 15.91767397667354089 ) ;
#5750 = VERTEX_POINT ( 'NONE', #4664 ) ;
#5751 = DIRECTION ( 'NONE',  ( 0.000000000000000000, 0.000000000000000000, 1.000000000000000000 ) ) ;
#5752 = DIRECTION ( 'NONE',  ( 0.000000000000000000, 0.000000000000000000, 1.000000000000000000 ) ) ;
#5753 = EDGE_LOOP ( 'NONE', ( #11316, #13208, #4839 ) ) ;
#5754 = VECTOR ( 'NONE', #1023, 1000.000000000000000 ) ;
#5755 = VERTEX_POINT ( 'NONE', #6206 ) ;
#5756 = EDGE_CURVE ( 'NONE', #18071, #5912, #14895, .T. ) ;
#5757 = EDGE_CURVE ( 'NONE', #16327, #16961, #10888, .T. ) ;
#5758 = ORIENTED_EDGE ( 'NONE', *, *, #10034, .T. ) ;
#5759 = EDGE_CURVE ( 'NONE', #8471, #13722, #15084, .T. ) ;
#5760 = CARTESIAN_POINT ( 'NONE',  ( -12.14914984460759584, -59.51523122377249564, 283.5832628385307999 ) ) ;
#5761 = ORIENTED_EDGE ( 'NONE', *, *, #11490, .T. ) ;
#5762 = FACE_OUTER_BOUND ( 'NONE', #5720, .T. ) ;
#5763 = AXIS2_PLACEMENT_3D ( 'NONE', #7515, #13957, #20200 ) ;
#5764 = CIRCLE ( 'NONE', #8053, 32.50000000000000000 ) ;
#5765 = FACE_OUTER_BOUND ( 'NONE', #14718, .T. ) ;
#5766 = CARTESIAN_POINT ( 'NONE',  ( -95.54273718347639033, -115.6434791701697833, 49.24035574262877901 ) ) ;
#5767 = DIRECTION ( 'NONE',  ( -1.000000000000000000, 0.000000000000000000, 0.000000000000000000 ) ) ;
#5768 = EDGE_LOOP ( 'NONE', ( #8935, #12879, #6123, #16032 ) ) ;
#5769 = DIRECTION ( 'NONE',  ( 1.000000000000000000, 0.000000000000000000, 0.000000000000000000 ) ) ;
#5770 = CARTESIAN_POINT ( 'NONE',  ( -132.3052566686612579, -70.67971788940300826, -3.041505667804067947 ) ) ;
#5771 = VECTOR ( 'NONE', #11203, 1000.000000000000227 ) ;
#5772 = EDGE_CURVE ( 'NONE', #16770, #20118, #4972, .T. ) ;
#5773 = CARTESIAN_POINT ( 'NONE',  ( 122.8001410695374602, -86.14014948502068592, -9.999999999999998224 ) ) ;
#5774 = CARTESIAN_POINT ( 'NONE',  ( 24.95276293194452322, -10.68636129284898573, 39.88498244535527704 ) ) ;
#5775 = CARTESIAN_POINT ( 'NONE',  ( -135.1060089022256818, -65.16414933467422088, 30.00000000000000711 ) ) ;
#5776 = ORIENTED_EDGE ( 'NONE', *, *, #1850, .F. ) ;
#5777 = CARTESIAN_POINT ( 'NONE',  ( 44.89578954330598748, 107.1965464310834477, 39.88498244535514203 ) ) ;
#5778 = CIRCLE ( 'NONE', #12293, 60.74260934110282051 ) ;
#5779 = VERTEX_POINT ( 'NONE', #9664 ) ;
#5780 = AXIS2_PLACEMENT_3D ( 'NONE', #6780, #18856, #9834 ) ;
#5781 = ORIENTED_EDGE ( 'NONE', *, *, #8019, .F. ) ;
#5782 = EDGE_CURVE ( 'NONE', #2184, #2170, #17208, .T. ) ;
#5783 = EDGE_CURVE ( 'NONE', #18061, #1300, #2490, .T. ) ;
#5784 = VERTEX_POINT ( 'NONE', #12929 ) ;
#5785 = TOROIDAL_SURFACE ( 'NONE', #17230, 110.0000000000000142, 40.00000000000000000 ) ;
#5786 = VERTEX_POINT ( 'NONE', #1589 ) ;
#5787 = EDGE_CURVE ( 'NONE', #15721, #13855, #14172, .T. ) ;
#5788 = DIRECTION ( 'NONE',  ( 0.9781142164131917394, -0.2080686897406911207, 0.000000000000000000 ) ) ;
#5789 = CARTESIAN_POINT ( 'NONE',  ( 0.000000000000000000, 0.000000000000000000, 283.5832628385307999 ) ) ;
#5790 = EDGE_LOOP ( 'NONE', ( #8970, #8483, #14543, #4606 ) ) ;
#5791 = CARTESIAN_POINT ( 'NONE',  ( -137.3668080473636053, -22.65449782367379328, -16.82459036858919177 ) ) ;
#5792 = DIRECTION ( 'NONE',  ( 0.000000000000000000, 0.000000000000000000, 1.000000000000000000 ) ) ;
#5793 = VERTEX_POINT ( 'NONE', #14573 ) ;
#5794 = CARTESIAN_POINT ( 'NONE',  ( 41.02350267428969488, 44.79940644582669051, 283.5832628385307999 ) ) ;
#5795 = CARTESIAN_POINT ( 'NONE',  ( 78.68887634719573043, -147.8252249328912740, 60.00000000000000000 ) ) ;
#5796 = FACE_OUTER_BOUND ( 'NONE', #16439, .T. ) ;
#5797 = CARTESIAN_POINT ( 'NONE',  ( -59.06449708980196078, -51.36153797460887915, 248.9926560891072143 ) ) ;
#5798 = VECTOR ( 'NONE', #2431, 1000.000000000000000 ) ;
#5799 = CARTESIAN_POINT ( 'NONE',  ( 28.94886449118905247, -53.40063514825087765, 283.5832628385307999 ) ) ;
#5800 = CARTESIAN_POINT ( 'NONE',  ( 36.99387960884163107, -48.17797692984175484, 293.5832628385307999 ) ) ;
#5801 = ORIENTED_EDGE ( 'NONE', *, *, #10832, .T. ) ;
#5802 = CARTESIAN_POINT ( 'NONE',  ( -156.4179374840092862, -52.02840013024096066, 39.99999999999999289 ) ) ;
#5803 = ORIENTED_EDGE ( 'NONE', *, *, #2057, .F. ) ;
#5804 = ORIENTED_EDGE ( 'NONE', *, *, #3125, .T. ) ;
#5805 = DIRECTION ( 'NONE',  ( -1.000000000000000000, 0.000000000000000000, 6.976128451377903642E-15 ) ) ;
#5806 = ORIENTED_EDGE ( 'NONE', *, *, #13128, .F. ) ;
#5807 = ORIENTED_EDGE ( 'NONE', *, *, #4277, .T. ) ;
#5808 = AXIS2_PLACEMENT_3D ( 'NONE', #1410, #12132, #18395 ) ;
#5809 = EDGE_CURVE ( 'NONE', #5313, #3073, #2303, .T. ) ;
#5810 = DIRECTION ( 'NONE',  ( 0.6234898018587433643, -0.7818314824680220321, 0.000000000000000000 ) ) ;
#5811 = AXIS2_PLACEMENT_3D ( 'NONE', #3912, #5648, #5084 ) ;
#5812 = DIRECTION ( 'NONE',  ( -0.000000000000000000, -0.000000000000000000, 1.000000000000000000 ) ) ;
#5813 = EDGE_LOOP ( 'NONE', ( #9608, #3071, #20007, #13407 ) ) ;
#5814 = DIRECTION ( 'NONE',  ( -0.000000000000000000, -0.000000000000000000, 1.000000000000000000 ) ) ;
#5815 = CARTESIAN_POINT ( 'NONE',  ( -20.74471755083563806, 59.39925916207565137, 248.9926560891072143 ) ) ;
#5816 = VERTEX_POINT ( 'NONE', #8724 ) ;
#5817 = CARTESIAN_POINT ( 'NONE',  ( -126.0117988550010182, -81.37275256441674287, 49.38489965504906110 ) ) ;
#5818 = CARTESIAN_POINT ( 'NONE',  ( 0.000000000000000000, 164.0736214083062805, 60.00000000000000000 ) ) ;
#5819 = LINE ( 'NONE', #9186, #817 ) ;
#5820 = ORIENTED_EDGE ( 'NONE', *, *, #15534, .T. ) ;
#5821 = CARTESIAN_POINT ( 'NONE',  ( 0.000000000000000000, 164.0736214083062805, 49.99999999999999289 ) ) ;
#5822 = CARTESIAN_POINT ( 'NONE',  ( -131.9731329243527682, -88.11278280481133152, 39.76642901553087484 ) ) ;
#5823 = CARTESIAN_POINT ( 'NONE',  ( 79.05640494598117129, -127.4758205975433327, 49.99999999999999289 ) ) ;
#5824 = AXIS2_PLACEMENT_3D ( 'NONE', #13749, #4342, #18264 ) ;
#5825 = ORIENTED_EDGE ( 'NONE', *, *, #11372, .T. ) ;
#5826 = VECTOR ( 'NONE', #12894, 1000.000000000000227 ) ;
#5827 = DIRECTION ( 'NONE',  ( -0.000000000000000000, -0.000000000000000000, 1.000000000000000000 ) ) ;
#5828 = DIRECTION ( 'NONE',  ( 0.000000000000000000, 0.000000000000000000, -1.000000000000000000 ) ) ;
#5829 = VERTEX_POINT ( 'NONE', #19382 ) ;
#5830 = ORIENTED_EDGE ( 'NONE', *, *, #15675, .F. ) ;
#5831 = CARTESIAN_POINT ( 'NONE',  ( -82.23581699221313102, -125.4482974261014192, 32.97002058077946174 ) ) ;
#5832 = VERTEX_POINT ( 'NONE', #13217 ) ;
#5833 = EDGE_CURVE ( 'NONE', #5755, #16770, #6417, .T. ) ;
#5834 = DIRECTION ( 'NONE',  ( -0.5300553768524346454, -0.8479630283625717579, 0.000000000000000000 ) ) ;
#5835 = CARTESIAN_POINT ( 'NONE',  ( -23.22718332831480481, -56.12853591711337486, 283.5832628385307999 ) ) ;
#5836 = VERTEX_POINT ( 'NONE', #10164 ) ;
#5837 = VECTOR ( 'NONE', #15163, 1000.000000000000000 ) ;
#5838 = DIRECTION ( 'NONE',  ( 1.000000000000000000, 0.000000000000000000, 0.000000000000000000 ) ) ;
#5839 = CARTESIAN_POINT ( 'NONE',  ( -98.08728810294334721, -113.5042871117647962, 1.876579804940954110 ) ) ;
#5840 = AXIS2_PLACEMENT_3D ( 'NONE', #18724, #18935, #12875 ) ;
#5841 = VECTOR ( 'NONE', #6028, 1000.000000000000227 ) ;
#5842 = CIRCLE ( 'NONE', #9768, 60.74260934110282051 ) ;
#5843 = DIRECTION ( 'NONE',  ( 0.6692498792541753394, 0.7430374143461900838, 0.000000000000000000 ) ) ;
#5844 = DIRECTION ( 'NONE',  ( 6.982962677686266711E-15, -0.000000000000000000, 1.000000000000000000 ) ) ;
#5845 = CARTESIAN_POINT ( 'NONE',  ( -30.53958573130872978, 50.13752642112859803, 110.9660488491356887 ) ) ;
#5846 = EDGE_CURVE ( 'NONE', #3935, #14265, #14961, .T. ) ;
#5847 = FACE_OUTER_BOUND ( 'NONE', #18651, .T. ) ;
#5848 = CARTESIAN_POINT ( 'NONE',  ( -29.92423416078134935, 37.80811387934245005, 248.9926560891072143 ) ) ;
#5849 = DIRECTION ( 'NONE',  ( -1.000000000000000000, 0.000000000000000000, 0.000000000000000000 ) ) ;
#5850 = CARTESIAN_POINT ( 'NONE',  ( 17.49999999999999289, 0.000000000000000000, 39.88498244535532677 ) ) ;
#5851 = ORIENTED_EDGE ( 'NONE', *, *, #12260, .F. ) ;
#5852 = CARTESIAN_POINT ( 'NONE',  ( 28.94983032429829350, -53.40245231972188833, 293.5832628385307999 ) ) ;
#5853 = CARTESIAN_POINT ( 'NONE',  ( -79.05640494597940915, -127.4758205975444270, 60.00000000000000000 ) ) ;
#5854 = CONICAL_SURFACE ( 'NONE', #17302, 79.75827554147308263, 0.5305858521701756203 ) ;
#5855 = ORIENTED_EDGE ( 'NONE', *, *, #12070, .T. ) ;
#5856 = VECTOR ( 'NONE', #14308, 1000.000000000000227 ) ;
#5857 = VECTOR ( 'NONE', #283, 1000.000000000000000 ) ;
#5858 = VECTOR ( 'NONE', #16218, 1000.000000000000227 ) ;
#5859 = ORIENTED_EDGE ( 'NONE', *, *, #4643, .F. ) ;
#5860 = EDGE_LOOP ( 'NONE', ( #13086, #7023, #7441, #11510 ) ) ;
#5861 = EDGE_CURVE ( 'NONE', #11829, #2786, #19801, .T. ) ;
#5862 = FACE_BOUND ( 'NONE', #11541, .T. ) ;
#5863 = ORIENTED_EDGE ( 'NONE', *, *, #11979, .T. ) ;
#5864 = FACE_OUTER_BOUND ( 'NONE', #7305, .T. ) ;
#5865 = CARTESIAN_POINT ( 'NONE',  ( 113.3640620605771261, -25.59923667990641150, 39.88498244535465886 ) ) ;
#5866 = FACE_OUTER_BOUND ( 'NONE', #19611, .T. ) ;
#5867 = CARTESIAN_POINT ( 'NONE',  ( 7.948937137877743808, -60.22232964560488000, 283.5832628385307999 ) ) ;
#5868 = LINE ( 'NONE', #1148, #10317 ) ;
#5869 = FACE_OUTER_BOUND ( 'NONE', #8321, .T. ) ;
#5870 = AXIS2_PLACEMENT_3D ( 'NONE', #18891, #4771, #12222 ) ;
#5871 = AXIS2_PLACEMENT_3D ( 'NONE', #6707, #351, #3726 ) ;
#5872 = ORIENTED_EDGE ( 'NONE', *, *, #11994, .T. ) ;
#5873 = CARTESIAN_POINT ( 'NONE',  ( 0.000000000000000000, 0.000000000000000000, 248.9926560891072143 ) ) ;
#5874 = CARTESIAN_POINT ( 'NONE',  ( -134.7264294273345797, -65.94569739564882127, 4.828444922764884240 ) ) ;
#5875 = EDGE_CURVE ( 'NONE', #3831, #219, #1360, .T. ) ;
#5876 = CARTESIAN_POINT ( 'NONE',  ( 132.0132531075724387, -71.33615934021467808, 3.697065622178481004 ) ) ;
#5877 = LINE ( 'NONE', #4434, #9520 ) ;
#5878 = FACE_OUTER_BOUND ( 'NONE', #17518, .T. ) ;
#5879 = CARTESIAN_POINT ( 'NONE',  ( -133.2712073793125569, -68.96827650305597501, 30.00000000000000000 ) ) ;
#5880 = ORIENTED_EDGE ( 'NONE', *, *, #9134, .T. ) ;
#5881 = EDGE_CURVE ( 'NONE', #818, #6064, #15891, .T. ) ;
#5882 = DIRECTION ( 'NONE',  ( 1.000000000000000000, 0.000000000000000000, -0.000000000000000000 ) ) ;
#5883 = ORIENTED_EDGE ( 'NONE', *, *, #6897, .T. ) ;
#5884 = ORIENTED_EDGE ( 'NONE', *, *, #16393, .F. ) ;
#5885 = EDGE_LOOP ( 'NONE', ( #13901, #17723, #12361 ) ) ;
#5886 = ADVANCED_FACE ( 'NONE', ( #4533 ), #8825, .F. ) ;
#5887 = VERTEX_POINT ( 'NONE', #13728 ) ;
#5888 = DIRECTION ( 'NONE',  ( 0.7406645559057084549, 0.6718749999999998890, -1.123343240388176004E-15 ) ) ;
#5889 = CARTESIAN_POINT ( 'NONE',  ( 38.78191089773071809, -44.07268132743684674, 132.4711112102474146 ) ) ;
#5890 = LINE ( 'NONE', #7312, #4862 ) ;
#5891 = ORIENTED_EDGE ( 'NONE', *, *, #16491, .T. ) ;
#5892 = CARTESIAN_POINT ( 'NONE',  ( 0.000000000000000000, 0.000000000000000000, 132.4711112102474146 ) ) ;
#5893 = DIRECTION ( 'NONE',  ( 0.000000000000000000, 0.000000000000000000, -1.000000000000000000 ) ) ;
#5894 = EDGE_LOOP ( 'NONE', ( #11916, #17425, #15032, #8904 ) ) ;
#5895 = CARTESIAN_POINT ( 'NONE',  ( 21.51662357877997422, -16.14275151819498078, 14.88498244535530191 ) ) ;
#5896 = AXIS2_PLACEMENT_3D ( 'NONE', #6340, #4700, #9398 ) ;
#5897 = FACE_OUTER_BOUND ( 'NONE', #20126, .T. ) ;
#5898 = DIRECTION ( 'NONE',  ( 0.4338837391175526248, 0.9009688679024218105, -0.000000000000000000 ) ) ;
#5899 = AXIS2_PLACEMENT_3D ( 'NONE', #948, #19572, #14962 ) ;
#5900 = ADVANCED_FACE ( 'NONE', ( #20076 ), #16610, .F. ) ;
#5901 = CIRCLE ( 'NONE', #16027, 7.500000000000006217 ) ;
#5902 = CARTESIAN_POINT ( 'NONE',  ( 144.1130761623740568, -69.50842595698583182, 30.00000000000000000 ) ) ;
#5903 = EDGE_CURVE ( 'NONE', #15182, #12589, #2902, .T. ) ;
#5904 = EDGE_CURVE ( 'NONE', #12139, #15302, #8922, .T. ) ;
#5905 = ADVANCED_FACE ( 'NONE', ( #9234 ), #11983, .F. ) ;
#5906 = CARTESIAN_POINT ( 'NONE',  ( 122.8001410695374886, -86.14014948502062907, 40.00000000000000711 ) ) ;
#5907 = CARTESIAN_POINT ( 'NONE',  ( 116.5881606921954017, -25.59923667990641150, 14.88498244535463755 ) ) ;
#5908 = ORIENTED_EDGE ( 'NONE', *, *, #2975, .F. ) ;
#5909 = ORIENTED_EDGE ( 'NONE', *, *, #10008, .F. ) ;
#5910 = DIRECTION ( 'NONE',  ( 6.982962677686266711E-15, -0.000000000000000000, 1.000000000000000000 ) ) ;
#5911 = VERTEX_POINT ( 'NONE', #7692 ) ;
#5912 = VERTEX_POINT ( 'NONE', #13937 ) ;
#5913 = FACE_OUTER_BOUND ( 'NONE', #2803, .T. ) ;
#5914 = VECTOR ( 'NONE', #2232, 1000.000000000000000 ) ;
#5915 = EDGE_CURVE ( 'NONE', #7860, #12583, #5868, .T. ) ;
#5916 = ORIENTED_EDGE ( 'NONE', *, *, #11954, .F. ) ;
#5917 = ORIENTED_EDGE ( 'NONE', *, *, #11967, .F. ) ;
#5918 = AXIS2_PLACEMENT_3D ( 'NONE', #7723, #13963, #3135 ) ;
#5919 = CARTESIAN_POINT ( 'NONE',  ( 60.00000000000000711, 6.284666409917639535E-13, -115.0000000000000000 ) ) ;
#5920 = CARTESIAN_POINT ( 'NONE',  ( 0.000000000000000000, 0.000000000000000000, 283.5832628385307999 ) ) ;
#5921 = CARTESIAN_POINT ( 'NONE',  ( -49.59485801383857506, -102.5175491340983882, 14.88498244535579929 ) ) ;
#5922 = ORIENTED_EDGE ( 'NONE', *, *, #340, .T. ) ;
#5923 = DIRECTION ( 'NONE',  ( -0.000000000000000000, -0.000000000000000000, -1.000000000000000000 ) ) ;
#5924 = CARTESIAN_POINT ( 'NONE',  ( 3.123743752084087610, -4.811834253409037920, 293.5832628385307999 ) ) ;
#5925 = ORIENTED_EDGE ( 'NONE', *, *, #7063, .F. ) ;
#5926 = CARTESIAN_POINT ( 'NONE',  ( 47.56406379474552182, 37.78325588002191893, 293.5832628385307999 ) ) ;
#5927 = DIRECTION ( 'NONE',  ( 0.1736481776669172583, 0.9848077530122103518, 0.000000000000000000 ) ) ;
#5928 = EDGE_CURVE ( 'NONE', #48, #2962, #133, .T. ) ;
#5929 = DIRECTION ( 'NONE',  ( 0.000000000000000000, 0.000000000000000000, -1.000000000000000000 ) ) ;
#5930 = VECTOR ( 'NONE', #20073, 1000.000000000000000 ) ;
#5931 = EDGE_LOOP ( 'NONE', ( #6221, #6036, #12966 ) ) ;
#5932 = LINE ( 'NONE', #10608, #3509 ) ;
#5933 = DIRECTION ( 'NONE',  ( -1.000000000000000000, 0.000000000000000000, 0.000000000000000000 ) ) ;
#5934 = CIRCLE ( 'NONE', #8540, 60.74260934110282051 ) ;
#5935 = CARTESIAN_POINT ( 'NONE',  ( -110.0000000000000142, 86.60254037844390496, 39.99999999999997868 ) ) ;
#5936 = EDGE_CURVE ( 'NONE', #9122, #9886, #7068, .T. ) ;
#5937 = ORIENTED_EDGE ( 'NONE', *, *, #6295, .T. ) ;
#5938 = FACE_BOUND ( 'NONE', #18985, .T. ) ;
#5939 = LINE ( 'NONE', #15330, #16449 ) ;
#5940 = ORIENTED_EDGE ( 'NONE', *, *, #6243, .T. ) ;
#5941 = ORIENTED_EDGE ( 'NONE', *, *, #10899, .T. ) ;
#5942 = CARTESIAN_POINT ( 'NONE',  ( -97.58310720701108210, -133.8455726501527181, 31.29999797859053956 ) ) ;
#5943 = VERTEX_POINT ( 'NONE', #12499 ) ;
#5944 = LINE ( 'NONE', #5537, #17321 ) ;
#5945 = CARTESIAN_POINT ( 'NONE',  ( 0.000000000000000000, 0.000000000000000000, -49.99999999999999289 ) ) ;
#5946 = ORIENTED_EDGE ( 'NONE', *, *, #13127, .F. ) ;
#5947 = CARTESIAN_POINT ( 'NONE',  ( -7.499999999999583444, -60.00000000000000000, -105.0000000000000142 ) ) ;
#5948 = FACE_OUTER_BOUND ( 'NONE', #18166, .T. ) ;
#5949 = CARTESIAN_POINT ( 'NONE',  ( -136.4619910415503625, -31.11745988142876129, -11.67418830189604328 ) ) ;
#5950 = DIRECTION ( 'NONE',  ( 0.7071067811865493491, 8.659560562354956277E-17, -0.7071067811865455743 ) ) ;
#5951 = FACE_BOUND ( 'NONE', #3302, .T. ) ;
#5952 = CARTESIAN_POINT ( 'NONE',  ( 0.000000000000000000, 0.000000000000000000, 248.9926560891072143 ) ) ;
#5953 = DIRECTION ( 'NONE',  ( -6.982962677686266711E-15, 0.000000000000000000, -1.000000000000000000 ) ) ;
#5954 = CARTESIAN_POINT ( 'NONE',  ( 84.12422660803940744, -124.1903156958371000, 39.21023289894657893 ) ) ;
#5955 = VERTEX_POINT ( 'NONE', #10020 ) ;
#5956 = FACE_OUTER_BOUND ( 'NONE', #18725, .T. ) ;
#5957 = DIRECTION ( 'NONE',  ( -0.000000000000000000, -0.000000000000000000, 1.000000000000000000 ) ) ;
#5958 = ORIENTED_EDGE ( 'NONE', *, *, #13101, .T. ) ;
#5959 = ORIENTED_EDGE ( 'NONE', *, *, #13228, .T. ) ;
#5960 = AXIS2_PLACEMENT_3D ( 'NONE', #16819, #4756, #10978 ) ;
#5961 = VECTOR ( 'NONE', #16019, 1000.000000000000000 ) ;
#5962 = VERTEX_POINT ( 'NONE', #3107 ) ;
#5963 = FACE_BOUND ( 'NONE', #5964, .T. ) ;
#5964 = EDGE_LOOP ( 'NONE', ( #7932, #18960, #19196 ) ) ;
#5965 = VECTOR ( 'NONE', #2380, 999.9999999999998863 ) ;
#5966 = CARTESIAN_POINT ( 'NONE',  ( 28.06680738835026290, -53.87178215532764369, 293.5832628385307999 ) ) ;
#5967 = LINE ( 'NONE', #19967, #4362 ) ;
#5968 = CARTESIAN_POINT ( 'NONE',  ( 0.000000000000000000, 0.000000000000000000, 49.99999999999999289 ) ) ;
#5969 = DIRECTION ( 'NONE',  ( -0.5742676632334714482, -0.8186676071302495528, 0.000000000000000000 ) ) ;
#5970 = DIRECTION ( 'NONE',  ( 0.000000000000000000, 0.000000000000000000, 1.000000000000000000 ) ) ;
#5971 = FACE_OUTER_BOUND ( 'NONE', #2488, .T. ) ;
#5972 = ORIENTED_EDGE ( 'NONE', *, *, #17806, .F. ) ;
#5973 = DIRECTION ( 'NONE',  ( 1.000000000000000000, 0.000000000000000000, 0.000000000000000000 ) ) ;
#5974 = CARTESIAN_POINT ( 'NONE',  ( -134.3415992761221105, -66.72651222969516027, 2.774043998594589056 ) ) ;
#5975 = CARTESIAN_POINT ( 'NONE',  ( 134.2478682171850437, -76.37034190854629401, 4.533283974515958548 ) ) ;
#5976 = VECTOR ( 'NONE', #18202, 1000.000000000000000 ) ;
#5977 = CIRCLE ( 'NONE', #10522, 7.500000000000012434 ) ;
#5978 = LINE ( 'NONE', #10560, #2338 ) ;
#5979 = CYLINDRICAL_SURFACE ( 'NONE', #19639, 7.500000000000020428 ) ;
#5980 = CARTESIAN_POINT ( 'NONE',  ( -135.0085555318103729, -65.36720921928038308, 33.00376037643530935 ) ) ;
#5981 = ADVANCED_FACE ( 'NONE', ( #12707 ), #2156, .T. ) ;
#5982 = ORIENTED_EDGE ( 'NONE', *, *, #11603, .F. ) ;
#5983 = FACE_OUTER_BOUND ( 'NONE', #14130, .T. ) ;
#5984 = CIRCLE ( 'NONE', #18068, 5.035999999999999588 ) ;
#5985 = ORIENTED_EDGE ( 'NONE', *, *, #17890, .T. ) ;
#5986 = ORIENTED_EDGE ( 'NONE', *, *, #12025, .F. ) ;
#5987 = EDGE_CURVE ( 'NONE', #3620, #6087, #1674, .T. ) ;
#5988 = AXIS2_PLACEMENT_3D ( 'NONE', #12458, #12360, #15545 ) ;
#5989 = VECTOR ( 'NONE', #19966, 1000.000000000000000 ) ;
#5990 = ORIENTED_EDGE ( 'NONE', *, *, #13629, .F. ) ;
#5991 = EDGE_CURVE ( 'NONE', #9376, #6851, #10864, .T. ) ;
#5992 = CARTESIAN_POINT ( 'NONE',  ( -138.8349868765292854, -24.00226663467886468, 24.84023710039527799 ) ) ;
#5993 = EDGE_CURVE ( 'NONE', #11053, #5734, #11071, .T. ) ;
#5994 = CARTESIAN_POINT ( 'NONE',  ( 79.75827554147308263, 0.000000000000000000, 132.4711112102474146 ) ) ;
#5995 = CYLINDRICAL_SURFACE ( 'NONE', #3847, 34.99999999999997868 ) ;
#5996 = ORIENTED_EDGE ( 'NONE', *, *, #5285, .F. ) ;
#5997 = DIRECTION ( 'NONE',  ( 1.000000000000000000, 0.000000000000000000, 0.000000000000000000 ) ) ;
#5998 = FACE_OUTER_BOUND ( 'NONE', #6522, .T. ) ;
#5999 = EDGE_LOOP ( 'NONE', ( #15306, #8570, #6730 ) ) ;
#6000 = LINE ( 'NONE', #9569, #7797 ) ;
#6001 = DIRECTION ( 'NONE',  ( 1.000000000000000000, 3.491481338843133355E-15, 0.000000000000000000 ) ) ;
#6002 = CARTESIAN_POINT ( 'NONE',  ( -134.4445132543467309, -75.00751837915889553, 5.690310535856665908 ) ) ;
#6003 = CARTESIAN_POINT ( 'NONE',  ( 19.23677882349201695, -57.61823435390814296, 293.5832628385307999 ) ) ;
#6004 = EDGE_CURVE ( 'NONE', #13843, #5526, #11453, .T. ) ;
#6005 = CIRCLE ( 'NONE', #17836, 7.500000000000000000 ) ;
#6006 = CARTESIAN_POINT ( 'NONE',  ( 130.9868171408399746, -91.88282611735534999, 40.00000000000000000 ) ) ;
#6007 = CYLINDRICAL_SURFACE ( 'NONE', #19493, 62.91752772691707207 ) ;
#6008 = ORIENTED_EDGE ( 'NONE', *, *, #3890, .F. ) ;
#6009 = VERTEX_POINT ( 'NONE', #18970 ) ;
#6010 = CARTESIAN_POINT ( 'NONE',  ( 32.50000000000000000, 3.980102097228897837E-15, -105.0000000000000142 ) ) ;
#6011 = ORIENTED_EDGE ( 'NONE', *, *, #7642, .T. ) ;
#6012 = AXIS2_PLACEMENT_3D ( 'NONE', #3001, #9230, #12291 ) ;
#6013 = ORIENTED_EDGE ( 'NONE', *, *, #4039, .F. ) ;
#6014 = CARTESIAN_POINT ( 'NONE',  ( -181.0783081749256667, -200.0000000000000853, 10.00000000000000178 ) ) ;
#6015 = AXIS2_PLACEMENT_3D ( 'NONE', #20225, #4579, #4471 ) ;
#6016 = ORIENTED_EDGE ( 'NONE', *, *, #2665, .F. ) ;
#6017 = ORIENTED_EDGE ( 'NONE', *, *, #2616, .T. ) ;
#6018 = EDGE_CURVE ( 'NONE', #16017, #2735, #17843, .T. ) ;
#6019 = EDGE_CURVE ( 'NONE', #15218, #14685, #8036, .T. ) ;
#6020 = CARTESIAN_POINT ( 'NONE',  ( 0.09252763182291320887, -6.914127053141824852, 6.024380653971842747 ) ) ;
#6021 = FACE_OUTER_BOUND ( 'NONE', #3658, .T. ) ;
#6022 = DIRECTION ( 'NONE',  ( -0.3420201433256630508, -0.9396926207859104263, -0.000000000000000000 ) ) ;
#6023 = EDGE_LOOP ( 'NONE', ( #16426, #16726, #343, #3323 ) ) ;
#6024 = DIRECTION ( 'NONE',  ( -0.000000000000000000, -0.000000000000000000, 1.000000000000000000 ) ) ;
#6025 = FACE_OUTER_BOUND ( 'NONE', #770, .T. ) ;
#6026 = VERTEX_POINT ( 'NONE', #1569 ) ;
#6027 = FACE_BOUND ( 'NONE', #5598, .T. ) ;
#6028 = DIRECTION ( 'NONE',  ( -0.9749279121818226201, -0.2225209339563185285, 0.000000000000000000 ) ) ;
#6029 = AXIS2_PLACEMENT_3D ( 'NONE', #16396, #2376, #5445 ) ;
#6030 = CARTESIAN_POINT ( 'NONE',  ( 0.000000000000000000, 0.000000000000000000, 132.4711112102474146 ) ) ;
#6031 = EDGE_CURVE ( 'NONE', #5360, #3019, #4745, .T. ) ;
#6032 = VECTOR ( 'NONE', #14986, 1000.000000000000000 ) ;
#6033 = FACE_OUTER_BOUND ( 'NONE', #6573, .T. ) ;
#6034 = DIRECTION ( 'NONE',  ( 0.9848077530122104628, -0.1736481776669172861, 0.000000000000000000 ) ) ;
#6035 = CARTESIAN_POINT ( 'NONE',  ( -36.99387960884161686, 48.17797692984174773, 293.5832628385307999 ) ) ;
#6036 = ORIENTED_EDGE ( 'NONE', *, *, #14975, .T. ) ;
#6037 = DIRECTION ( 'NONE',  ( -1.000000000000000000, 0.000000000000000000, 0.000000000000000000 ) ) ;
#6038 = LINE ( 'NONE', #15225, #17765 ) ;
#6039 = VERTEX_POINT ( 'NONE', #14045 ) ;
#6040 = EDGE_LOOP ( 'NONE', ( #11606, #3123, #3055, #13266 ) ) ;
#6041 = DIRECTION ( 'NONE',  ( -0.000000000000000000, -0.000000000000000000, 1.000000000000000000 ) ) ;
#6042 = EDGE_CURVE ( 'NONE', #19700, #18461, #1772, .T. ) ;
#6043 = AXIS2_PLACEMENT_3D ( 'NONE', #19530, #2351, #8584 ) ;
#6044 = ORIENTED_EDGE ( 'NONE', *, *, #8529, .T. ) ;
#6045 = EDGE_CURVE ( 'NONE', #19232, #9109, #3680, .T. ) ;
#6046 = CARTESIAN_POINT ( 'NONE',  ( -5.590028426173819120, -1.289614712049182987, 283.5832628385307999 ) ) ;
#6047 = LINE ( 'NONE', #10731, #2724 ) ;
#6048 = ORIENTED_EDGE ( 'NONE', *, *, #2030, .F. ) ;
#6049 = CARTESIAN_POINT ( 'NONE',  ( 82.18707601317576916, -125.4802243595265736, 7.400004042823632666 ) ) ;
#6050 = DIRECTION ( 'NONE',  ( 1.000000000000000000, 0.000000000000000000, 0.000000000000000000 ) ) ;
#6051 = EDGE_CURVE ( 'NONE', #2942, #11211, #2252, .T. ) ;
#6052 = ADVANCED_FACE ( 'NONE', ( #17708 ), #14146, .F. ) ;
#6053 = VECTOR ( 'NONE', #1950, 1000.000000000000114 ) ;
#6054 = LINE ( 'NONE', #15046, #5253 ) ;
#6055 = DIRECTION ( 'NONE',  ( 0.8830229359480271656, 0.4693298356057563625, 0.000000000000000000 ) ) ;
#6056 = DIRECTION ( 'NONE',  ( -6.982962677686266711E-15, -3.944304526105059027E-31, -1.000000000000000000 ) ) ;
#6057 = AXIS2_PLACEMENT_3D ( 'NONE', #6030, #16760, #2751 ) ;
#6058 = CARTESIAN_POINT ( 'NONE',  ( -109.9999999999983515, 275.0000000000000000, 85.00000000000001421 ) ) ;
#6059 = DIRECTION ( 'NONE',  ( -1.000000000000000000, 0.000000000000000000, 6.456589605409171438E-15 ) ) ;
#6060 = CARTESIAN_POINT ( 'NONE',  ( 101.4383890160197126, -128.4709723833431383, 37.98072183278354430 ) ) ;
#6061 = ORIENTED_EDGE ( 'NONE', *, *, #6591, .F. ) ;
#6062 = DIRECTION ( 'NONE',  ( 0.000000000000000000, 0.000000000000000000, -1.000000000000000000 ) ) ;
#6063 = LINE ( 'NONE', #12068, #5008 ) ;
#6064 = VERTEX_POINT ( 'NONE', #6183 ) ;
#6065 = ORIENTED_EDGE ( 'NONE', *, *, #8721, .T. ) ;
#6066 = DIRECTION ( 'NONE',  ( 1.000000000000000000, 0.000000000000000000, -3.491481338843133355E-15 ) ) ;
#6067 =( GEOMETRIC_REPRESENTATION_CONTEXT ( 3 ) GLOBAL_UNCERTAINTY_ASSIGNED_CONTEXT ( ( #4353 ) ) GLOBAL_UNIT_ASSIGNED_CONTEXT ( ( #8097, #9837, #17534 ) ) REPRESENTATION_CONTEXT ( 'NONE', 'WORKASPACE' ) );
#6068 = ORIENTED_EDGE ( 'NONE', *, *, #18801, .T. ) ;
#6069 = DIRECTION ( 'NONE',  ( 0.2080686897406943681, 0.9781142164131909622, 0.000000000000000000 ) ) ;
#6070 = VERTEX_POINT ( 'NONE', #9547 ) ;
#6071 = LINE ( 'NONE', #9543, #4679 ) ;
#6072 = DIRECTION ( 'NONE',  ( -6.982962677686266711E-15, 0.000000000000000000, -1.000000000000000000 ) ) ;
#6073 = DIRECTION ( 'NONE',  ( 0.000000000000000000, 0.000000000000000000, 1.000000000000000000 ) ) ;
#6074 = CARTESIAN_POINT ( 'NONE',  ( -107.4999999999999716, -118.5063289449133777, 40.00000000000000711 ) ) ;
#6075 = DIRECTION ( 'NONE',  ( -0.7881095627315619634, -0.6155349844899687950, 0.000000000000000000 ) ) ;
#6076 = FACE_OUTER_BOUND ( 'NONE', #13508, .T. ) ;
#6077 = VECTOR ( 'NONE', #13144, 1000.000000000000227 ) ;
#6078 = FACE_OUTER_BOUND ( 'NONE', #14539, .T. ) ;
#6079 = CARTESIAN_POINT ( 'NONE',  ( -134.7130977013099198, -72.98159303034539391, 9.251533979818299613 ) ) ;
#6080 = CARTESIAN_POINT ( 'NONE',  ( 133.6156149914907303, -80.24737158797387337, 2.358024411017839661 ) ) ;
#6081 = DIRECTION ( 'NONE',  ( 0.000000000000000000, 0.000000000000000000, 1.000000000000000000 ) ) ;
#6082 = VECTOR ( 'NONE', #15424, 1000.000000000000114 ) ;
#6083 = CARTESIAN_POINT ( 'NONE',  ( -63.68887634719364144, -147.8252249328922687, 60.00000000000000000 ) ) ;
#6084 = CARTESIAN_POINT ( 'NONE',  ( -129.7375433114042096, -75.28992114163499139, 46.76778812272521435 ) ) ;
#6085 = VERTEX_POINT ( 'NONE', #5318 ) ;
#6086 = DIRECTION ( 'NONE',  ( -1.000000000000000000, 0.000000000000000000, 0.000000000000000000 ) ) ;
#6087 = VERTEX_POINT ( 'NONE', #10967 ) ;
#6088 = VECTOR ( 'NONE', #15603, 1000.000000000000114 ) ;
#6089 = ORIENTED_EDGE ( 'NONE', *, *, #7902, .T. ) ;
#6090 = VECTOR ( 'NONE', #13617, 1000.000000000000227 ) ;
#6091 = ORIENTED_EDGE ( 'NONE', *, *, #11766, .T. ) ;
#6092 = EDGE_CURVE ( 'NONE', #13307, #6254, #8005, .T. ) ;
#6093 = VECTOR ( 'NONE', #1341, 999.9999999999998863 ) ;
#6094 = PLANE ( 'NONE',  #7006 ) ;
#6095 = CARTESIAN_POINT ( 'NONE',  ( -15.91767397667354800, 149.1530343478547422, 49.99999999999999289 ) ) ;
#6096 = ORIENTED_EDGE ( 'NONE', *, *, #242, .T. ) ;
#6097 = CARTESIAN_POINT ( 'NONE',  ( -135.6462056290698968, -28.96440493867737587, -18.85007980121054771 ) ) ;
#6098 = DIRECTION ( 'NONE',  ( 1.000000000000000000, 0.000000000000000000, 0.000000000000000000 ) ) ;
#6099 = ORIENTED_EDGE ( 'NONE', *, *, #4033, .T. ) ;
#6100 = CARTESIAN_POINT ( 'NONE',  ( 1.379293853801755176, -58.69016442926522359, 132.4711112102474146 ) ) ;
#6101 = CYLINDRICAL_SURFACE ( 'NONE', #16405, 106.4288957539801004 ) ;
#6102 = CARTESIAN_POINT ( 'NONE',  ( 39.84224160888901167, 67.36461649554546227, 248.9926560891072143 ) ) ;
#6103 = CARTESIAN_POINT ( 'NONE',  ( -38.41834839689332171, 68.18670162478844077, 248.9926560891072143 ) ) ;
#6104 = DIRECTION ( 'NONE',  ( 0.6427876096865379196, 0.7660444431189792347, 0.000000000000000000 ) ) ;
#6105 = VECTOR ( 'NONE', #6732, 1000.000000000000000 ) ;
#6106 = CIRCLE ( 'NONE', #20147, 60.74260934110282051 ) ;
#6107 = ADVANCED_FACE ( 'NONE', ( #229 ), #9919, .T. ) ;
#6108 = CARTESIAN_POINT ( 'NONE',  ( 133.2472142827512869, -69.01451035582651627, 31.05647528840589544 ) ) ;
#6109 = CARTESIAN_POINT ( 'NONE',  ( -176.7850001792984926, -190.0000000000000284, 33.42750952962406075 ) ) ;
#6110 = VERTEX_POINT ( 'NONE', #7053 ) ;
#6111 = ADVANCED_FACE ( 'NONE', ( #2347 ), #2447, .F. ) ;
#6113 = ORIENTED_EDGE ( 'NONE', *, *, #5534, .F. ) ;
#6112 = CIRCLE ( 'NONE', #5459, 62.91752772691707207 ) ;
#6114 = VERTEX_POINT ( 'NONE', #8678 ) ;
#6115 = VERTEX_POINT ( 'NONE', #13170 ) ;
#6116 = LINE ( 'NONE', #7938, #8282 ) ;
#6117 = EDGE_LOOP ( 'NONE', ( #3522, #13539, #15252, #4438, #4343, #1577 ) ) ;
#6118 = ORIENTED_EDGE ( 'NONE', *, *, #19057, .F. ) ;
#6119 = EDGE_CURVE ( 'NONE', #2886, #10466, #5778, .T. ) ;
#6120 = LINE ( 'NONE', #12335, #8446 ) ;
#6121 = DIRECTION ( 'NONE',  ( 0.000000000000000000, 0.000000000000000000, 1.000000000000000000 ) ) ;
#6122 = CARTESIAN_POINT ( 'NONE',  ( -78.26059000578311498, 0.8220851292432594937, 248.9926560891072143 ) ) ;
#6123 = ORIENTED_EDGE ( 'NONE', *, *, #17109, .T. ) ;
#6124 = CARTESIAN_POINT ( 'NONE',  ( -150.0000000000000284, 0.000000000000000000, 49.99999999999999289 ) ) ;
#6125 = CARTESIAN_POINT ( 'NONE',  ( -150.0000000000000284, 0.000000000000000000, 60.00000000000000000 ) ) ;
#6126 = EDGE_LOOP ( 'NONE', ( #14321, #7042, #6699, #18204 ) ) ;
#6127 = AXIS2_PLACEMENT_3D ( 'NONE', #5821, #13577, #12042 ) ;
#6128 = VECTOR ( 'NONE', #7701, 1000.000000000000000 ) ;
#6129 = CARTESIAN_POINT ( 'NONE',  ( -87.10655032386719654, -147.8252249328922687, 60.00000000000000000 ) ) ;
#6130 = CARTESIAN_POINT ( 'NONE',  ( 55.62246070845780110, -18.77710619359098132, 111.4180192758974499 ) ) ;
#6131 = CARTESIAN_POINT ( 'NONE',  ( 53.86996498385654064, 28.06584155524121016, 283.5832628385307999 ) ) ;
#6132 = EDGE_CURVE ( 'NONE', #7965, #17276, #3171, .T. ) ;
#6133 = LINE ( 'NONE', #18197, #16265 ) ;
#6134 = EDGE_CURVE ( 'NONE', #17581, #19621, #19821, .T. ) ;
#6135 = CARTESIAN_POINT ( 'NONE',  ( -134.5348546532066223, -74.34984901039666738, 33.58727947796721480 ) ) ;
#6136 = CARTESIAN_POINT ( 'NONE',  ( -92.45893247793782166, 105.1283412284861214, 35.29463395659252711 ) ) ;
#6137 = VERTEX_POINT ( 'NONE', #13268 ) ;
#6138 = DIRECTION ( 'NONE',  ( -0.000000000000000000, -0.000000000000000000, 1.000000000000000000 ) ) ;
#6139 = DIRECTION ( 'NONE',  ( 0.5000000000000044409, 0.8660254037844360431, -3.228294802704586902E-15 ) ) ;
#6140 = ORIENTED_EDGE ( 'NONE', *, *, #15206, .T. ) ;
#6141 = AXIS2_PLACEMENT_3D ( 'NONE', #13675, #15526, #1511 ) ;
#6142 = ORIENTED_EDGE ( 'NONE', *, *, #5140, .T. ) ;
#6143 = LINE ( 'NONE', #19939, #11696 ) ;
#6144 = VECTOR ( 'NONE', #19755, 1000.000000000000114 ) ;
#6145 = AXIS2_PLACEMENT_3D ( 'NONE', #19580, #2406, #857 ) ;
#6146 = EDGE_LOOP ( 'NONE', ( #15150, #767, #17767, #12532 ) ) ;
#6147 = LINE ( 'NONE', #12366, #5547 ) ;
#6148 = ADVANCED_FACE ( 'NONE', ( #1000 ), #10209, .T. ) ;
#6149 = LINE ( 'NONE', #16880, #12184 ) ;
#6150 = ORIENTED_EDGE ( 'NONE', *, *, #8297, .T. ) ;
#6151 = DIRECTION ( 'NONE',  ( -0.000000000000000000, -0.000000000000000000, 1.000000000000000000 ) ) ;
#6152 = CARTESIAN_POINT ( 'NONE',  ( 0.000000000000000000, 0.000000000000000000, 283.5832628385307999 ) ) ;
#6153 = CIRCLE ( 'NONE', #10060, 7.500000000000008882 ) ;
#6154 = CARTESIAN_POINT ( 'NONE',  ( -110.0000000000000142, 275.0000000000000000, -75.00000000000000000 ) ) ;
#6155 = CARTESIAN_POINT ( 'NONE',  ( -26.42151830275497915, 4.658826548058537576, 39.88498244535563941 ) ) ;
#6156 = AXIS2_PLACEMENT_3D ( 'NONE', #16380, #2167, #3981 ) ;
#6157 = ORIENTED_EDGE ( 'NONE', *, *, #4364, .F. ) ;
#6158 = CARTESIAN_POINT ( 'NONE',  ( -12.14957802882752524, -59.51724408343569905, 293.5832628385307999 ) ) ;
#6159 = EDGE_CURVE ( 'NONE', #8624, #15754, #14819, .T. ) ;
#6160 = DIRECTION ( 'NONE',  ( -0.6427876096865328126, -0.7660444431189835646, 0.000000000000000000 ) ) ;
#6161 = EDGE_CURVE ( 'NONE', #18071, #11232, #17856, .T. ) ;
#6162 = DIRECTION ( 'NONE',  ( -1.000000000000000000, 0.000000000000000000, -0.000000000000000000 ) ) ;
#6163 = CARTESIAN_POINT ( 'NONE',  ( 91.90390622750021521, -118.5498891763774481, 47.62726813621947741 ) ) ;
#6164 = ORIENTED_EDGE ( 'NONE', *, *, #8028, .T. ) ;
#6165 = EDGE_CURVE ( 'NONE', #15505, #16710, #19622, .T. ) ;
#6166 = PLANE ( 'NONE',  #19848 ) ;
#6167 = LINE ( 'NONE', #16794, #19685 ) ;
#6168 = ORIENTED_EDGE ( 'NONE', *, *, #7875, .F. ) ;
#6169 = ORIENTED_EDGE ( 'NONE', *, *, #348, .F. ) ;
#6170 = APPLICATION_PROTOCOL_DEFINITION ( 'draft international standard', 'automotive_design', 1998, #18620 ) ;
#6171 = VECTOR ( 'NONE', #2539, 1000.000000000000000 ) ;
#6172 = VECTOR ( 'NONE', #1112, 1000.000000000000000 ) ;
#6173 = ORIENTED_EDGE ( 'NONE', *, *, #3510, .F. ) ;
#6174 = VECTOR ( 'NONE', #11552, 1000.000000000000000 ) ;
#6175 = FACE_OUTER_BOUND ( 'NONE', #11130, .T. ) ;
#6176 = AXIS2_PLACEMENT_3D ( 'NONE', #5669, #3926, #755 ) ;
#6177 = FACE_BOUND ( 'NONE', #8793, .T. ) ;
#6178 = ORIENTED_EDGE ( 'NONE', *, *, #1420, .T. ) ;
#6179 = CARTESIAN_POINT ( 'NONE',  ( -159.9599531637108782, -36.50981547337168109, 39.99999999999999289 ) ) ;
#6180 = DIRECTION ( 'NONE',  ( 0.03505990758545895342, 0.9993852124581886764, 0.000000000000000000 ) ) ;
#6181 = CARTESIAN_POINT ( 'NONE',  ( 135.0831964404852954, -65.21150773178307247, 31.46019346751870316 ) ) ;
#6182 = CARTESIAN_POINT ( 'NONE',  ( -103.5848300920826688, -125.1657093462234229, 39.20674415995744511 ) ) ;
#6183 = CARTESIAN_POINT ( 'NONE',  ( 71.65703592476599226, -89.51573765728305432, 14.88498244535495196 ) ) ;
#6184 = DIRECTION ( 'NONE',  ( 0.3420201433256694901, -0.9396926207859082059, -0.000000000000000000 ) ) ;
#6185 = CARTESIAN_POINT ( 'NONE',  ( -58.63718168490499494, -22.81000261549349162, 132.4711112102474146 ) ) ;
#6186 = DIRECTION ( 'NONE',  ( -1.000000000000000000, 0.000000000000000000, 0.000000000000000000 ) ) ;
#6187 = CARTESIAN_POINT ( 'NONE',  ( 124.7133609680326032, -83.36099555804651118, -0.8783870393142805266 ) ) ;
#6188 = EDGE_CURVE ( 'NONE', #10259, #12149, #14597, .T. ) ;
#6189 = DIRECTION ( 'NONE',  ( 0.000000000000000000, 0.000000000000000000, -1.000000000000000000 ) ) ;
#6190 = DIRECTION ( 'NONE',  ( 0.3427509529624101492, -0.9394263059140720573, -0.000000000000000000 ) ) ;
#6191 = VECTOR ( 'NONE', #17880, 1000.000000000000000 ) ;
#6192 = CARTESIAN_POINT ( 'NONE',  ( -134.3546152455176355, -75.63949198389248352, 34.87809301592528755 ) ) ;
#6193 = CIRCLE ( 'NONE', #628, 62.91752772691707207 ) ;
#6194 = ORIENTED_EDGE ( 'NONE', *, *, #13642, .T. ) ;
#6195 = AXIS2_PLACEMENT_3D ( 'NONE', #4025, #19385, #5372 ) ;
#6196 = LINE ( 'NONE', #15382, #7266 ) ;
#6197 = EDGE_CURVE ( 'NONE', #9011, #14411, #8776, .T. ) ;
#6198 = EDGE_LOOP ( 'NONE', ( #3268, #14054, #11908, #2381 ) ) ;
#6199 = EDGE_LOOP ( 'NONE', ( #15926, #2250, #9115, #15038, #12898, #10732, #18439, #9436, #15076, #17218 ) ) ;
#6200 = ORIENTED_EDGE ( 'NONE', *, *, #2169, .F. ) ;
#6201 = AXIS2_PLACEMENT_3D ( 'NONE', #8229, #18995, #3636 ) ;
#6202 = CIRCLE ( 'NONE', #12388, 42.50000000000000000 ) ;
#6203 = LINE ( 'NONE', #6403, #20067 ) ;
#6204 = DIRECTION ( 'NONE',  ( 0.000000000000000000, 0.000000000000000000, 1.000000000000000000 ) ) ;
#6205 = VERTEX_POINT ( 'NONE', #16663 ) ;
#6206 = CARTESIAN_POINT ( 'NONE',  ( -85.53020504959707182, -140.9188050298390067, 39.99999999999999289 ) ) ;
#6207 = DIRECTION ( 'NONE',  ( -0.9271237148521536131, 0.3747554100459959958, 0.000000000000000000 ) ) ;
#6208 = EDGE_LOOP ( 'NONE', ( #10001, #1526, #4594, #15078 ) ) ;
#6209 = CARTESIAN_POINT ( 'NONE',  ( -103.2107452891376198, 83.78616291780149083, -29.34215614146094353 ) ) ;
#6210 = CARTESIAN_POINT ( 'NONE',  ( -2.629250726500700353, -60.68567895461850981, 293.5832628385307999 ) ) ;
#6211 = CARTESIAN_POINT ( 'NONE',  ( 92.34802049131684498, -66.64338626758360817, 14.88498244535480630 ) ) ;
#6212 = DIRECTION ( 'NONE',  ( 6.982962677686266711E-15, -0.000000000000000000, 1.000000000000000000 ) ) ;
#6213 = CARTESIAN_POINT ( 'NONE',  ( 60.08127757648377099, 8.938941455415205795, 283.5832628385307999 ) ) ;
#6214 = CARTESIAN_POINT ( 'NONE',  ( 135.1060089021447368, -65.16414933484200844, 30.74984108339598876 ) ) ;
#6215 = DIRECTION ( 'NONE',  ( -6.982962677686266711E-15, 0.000000000000000000, -1.000000000000000000 ) ) ;
#6216 = CIRCLE ( 'NONE', #16012, 77.50000000000000000 ) ;
#6217 = ORIENTED_EDGE ( 'NONE', *, *, #16687, .T. ) ;
#6218 = EDGE_CURVE ( 'NONE', #2611, #12822, #707, .T. ) ;
#6219 = ORIENTED_EDGE ( 'NONE', *, *, #14487, .T. ) ;
#6220 = ORIENTED_EDGE ( 'NONE', *, *, #6550, .T. ) ;
#6221 = ORIENTED_EDGE ( 'NONE', *, *, #17739, .T. ) ;
#6222 = DIRECTION ( 'NONE',  ( -0.000000000000000000, -0.000000000000000000, -1.000000000000000000 ) ) ;
#6223 = VERTEX_POINT ( 'NONE', #16860 ) ;
#6224 = PLANE ( 'NONE',  #15230 ) ;
#6225 = DIRECTION ( 'NONE',  ( -1.000000000000000000, -0.000000000000000000, -0.000000000000000000 ) ) ;
#6226 = VECTOR ( 'NONE', #7550, 1000.000000000000227 ) ;
#6227 = EDGE_CURVE ( 'NONE', #11122, #8663, #18498, .T. ) ;
#6228 = DIRECTION ( 'NONE',  ( 0.7430374143461878633, -0.6692498792541777819, 0.000000000000000000 ) ) ;
#6229 = DIRECTION ( 'NONE',  ( -1.000000000000000000, -0.000000000000000000, -0.000000000000000000 ) ) ;
#6230 = VERTEX_POINT ( 'NONE', #6129 ) ;
#6231 = AXIS2_PLACEMENT_3D ( 'NONE', #4536, #3007, #7696 ) ;
#6232 = DIRECTION ( 'NONE',  ( -0.1736481776669273613, 0.9848077530122085754, 1.206153050004590706E-15 ) ) ;
#6233 = DIRECTION ( 'NONE',  ( -0.000000000000000000, -0.000000000000000000, 1.000000000000000000 ) ) ;
#6234 = ORIENTED_EDGE ( 'NONE', *, *, #17892, .F. ) ;
#6235 = UNCERTAINTY_MEASURE_WITH_UNIT (LENGTH_MEASURE( 1.000000000000000082E-05 ), #13510, 'distance_accuracy_value', 'NONE');
#6236 = CARTESIAN_POINT ( 'NONE',  ( -72.91900756452172061, 131.0832496385607158, -10.00000000000000178 ) ) ;
#6237 = LINE ( 'NONE', #3262, #3879 ) ;
#6238 = CARTESIAN_POINT ( 'NONE',  ( -59.30716253403183202, 13.12726406102060217, 283.5832628385307999 ) ) ;
#6239 = PLANE ( 'NONE',  #7748 ) ;
#6240 = CARTESIAN_POINT ( 'NONE',  ( 134.1130761623740568, -69.50842595698583182, 30.00000000000000000 ) ) ;
#6241 = CYLINDRICAL_SURFACE ( 'NONE', #13143, 15.91767397667354089 ) ;
#6242 = ORIENTED_EDGE ( 'NONE', *, *, #17738, .T. ) ;
#6243 = EDGE_CURVE ( 'NONE', #3335, #720, #13988, .T. ) ;
#6244 = EDGE_CURVE ( 'NONE', #18601, #321, #7545, .T. ) ;
#6245 = PLANE ( 'NONE',  #19396 ) ;
#6246 = VERTEX_POINT ( 'NONE', #4377 ) ;
#6247 = AXIS2_PLACEMENT_3D ( 'NONE', #6612, #8133, #16222 ) ;
#6248 = ORIENTED_EDGE ( 'NONE', *, *, #7466, .F. ) ;
#6249 = DIRECTION ( 'NONE',  ( 1.000000000000000000, 0.000000000000000000, 0.000000000000000000 ) ) ;
#6250 = ORIENTED_EDGE ( 'NONE', *, *, #493, .T. ) ;
#6251 = CARTESIAN_POINT ( 'NONE',  ( -148.9554720520392834, -17.67108784863415138, 60.00000000000000000 ) ) ;
#6252 = EDGE_CURVE ( 'NONE', #18601, #1451, #10814, .T. ) ;
#6253 = DIRECTION ( 'NONE',  ( -1.000000000000000000, 0.000000000000000000, 0.000000000000000000 ) ) ;
#6254 = VERTEX_POINT ( 'NONE', #7646 ) ;
#6255 = ADVANCED_FACE ( 'NONE', ( #4480 ), #3261, .F. ) ;
#6256 = CARTESIAN_POINT ( 'NONE',  ( 82.35314629726865121, -125.3713054028912950, 6.290984962544095005 ) ) ;
#6257 = PLANE ( 'NONE',  #15556 ) ;
#6258 = EDGE_CURVE ( 'NONE', #3366, #10253, #15903, .T. ) ;
#6259 = VECTOR ( 'NONE', #18274, 1000.000000000000000 ) ;
#6260 = PLANE ( 'NONE',  #4583 ) ;
#6261 = PLANE ( 'NONE',  #9294 ) ;
#6262 = EDGE_LOOP ( 'NONE', ( #8217, #15103, #2688, #17395 ) ) ;
#6263 = CARTESIAN_POINT ( 'NONE',  ( 8.938941455415006843, -60.08127757648380651, 283.5832628385307999 ) ) ;
#6264 = CARTESIAN_POINT ( 'NONE',  ( -97.77191798235051579, 62.82820655979934088, 14.88498244535613502 ) ) ;
#6265 = DIRECTION ( 'NONE',  ( 0.000000000000000000, 0.000000000000000000, 1.000000000000000000 ) ) ;
#6266 = CARTESIAN_POINT ( 'NONE',  ( 99.06221739375077107, -131.8607669219688887, 35.36983001673655025 ) ) ;
#6267 = VERTEX_POINT ( 'NONE', #3059 ) ;
#6268 = ADVANCED_FACE ( 'NONE', ( #2852, #9077, #2956, #6027, #15214, #12346 ), #13887, .F. ) ;
#6269 = SHAPE_REPRESENTATION ( 'Base Flange', ( #18639 ), #3610 ) ;
#6270 = EDGE_CURVE ( 'NONE', #18758, #13055, #20233, .T. ) ;
#6271 = CARTESIAN_POINT ( 'NONE',  ( 68.18670162478807129, 38.41834839689403935, 132.4711112102474146 ) ) ;
#6272 = DIRECTION ( 'NONE',  ( -0.9271237148521536131, 0.3747554100459959958, 0.000000000000000000 ) ) ;
#6273 = VERTEX_POINT ( 'NONE', #16965 ) ;
#6274 = ORIENTED_EDGE ( 'NONE', *, *, #12340, .F. ) ;
#6275 = EDGE_LOOP ( 'NONE', ( #12357, #11702, #1808, #18130 ) ) ;
#6276 =( NAMED_UNIT ( * ) SI_UNIT ( $, .STERADIAN. ) SOLID_ANGLE_UNIT ( ) );
#6277 = ORIENTED_EDGE ( 'NONE', *, *, #13465, .F. ) ;
#6278 = CARTESIAN_POINT ( 'NONE',  ( -98.69444885161524894, -132.3639744934813791, 5.244265984552241910 ) ) ;
#6279 = LINE ( 'NONE', #4737, #19813 ) ;
#6280 = ORIENTED_EDGE ( 'NONE', *, *, #16624, .T. ) ;
#6281 = EDGE_CURVE ( 'NONE', #6717, #12028, #9019, .T. ) ;
#6282 = CARTESIAN_POINT ( 'NONE',  ( 48.17959877923549072, 36.99514631729036296, 293.5832628385307999 ) ) ;
#6283 = CARTESIAN_POINT ( 'NONE',  ( -1.629937663769596368, -60.72279549541552512, 293.5832628385307999 ) ) ;
#6284 = DIRECTION ( 'NONE',  ( -0.000000000000000000, -0.000000000000000000, 1.000000000000000000 ) ) ;
#6285 = EDGE_CURVE ( 'NONE', #17700, #8237, #1519, .T. ) ;
#6286 = EDGE_CURVE ( 'NONE', #10224, #65, #4668, .T. ) ;
#6287 = CARTESIAN_POINT ( 'NONE',  ( -103.8658874392065599, -124.7161237612890687, 39.32103072359011264 ) ) ;
#6288 = CARTESIAN_POINT ( 'NONE',  ( 27.90514497005375461, -110.4119590718113244, 14.88498244535525750 ) ) ;
#6289 = CARTESIAN_POINT ( 'NONE',  ( -118.0540516568924545, 75.28054536010147046, 39.07880203530302765 ) ) ;
#6290 = LINE ( 'NONE', #136, #8230 ) ;
#6291 = LINE ( 'NONE', #7597, #5279 ) ;
#6292 = CARTESIAN_POINT ( 'NONE',  ( -28.06584155524100765, 53.86996498385663301, 283.5832628385307999 ) ) ;
#6293 = CARTESIAN_POINT ( 'NONE',  ( -128.4532923017889345, -77.52586173742388098, 40.42418673595172862 ) ) ;
#6294 = ORIENTED_EDGE ( 'NONE', *, *, #6270, .F. ) ;
#6295 = EDGE_CURVE ( 'NONE', #8175, #9508, #14503, .T. ) ;
#6296 = PLANE ( 'NONE',  #5960 ) ;
#6297 = CIRCLE ( 'NONE', #9205, 112.8770930172170495 ) ;
#6298 = ORIENTED_EDGE ( 'NONE', *, *, #19958, .T. ) ;
#6299 = ORIENTED_EDGE ( 'NONE', *, *, #7107, .F. ) ;
#6300 = EDGE_LOOP ( 'NONE', ( #12339, #4522, #7710, #14563 ) ) ;
#6301 = ADVANCED_FACE ( 'NONE', ( #17484 ), #8054, .F. ) ;
#6302 = ADVANCED_FACE ( 'NONE', ( #17587 ), #1716, .T. ) ;
#6303 = DIRECTION ( 'NONE',  ( 0.000000000000000000, 0.000000000000000000, 1.000000000000000000 ) ) ;
#6304 = VECTOR ( 'NONE', #2914, 1000.000000000000000 ) ;
#6305 = DIRECTION ( 'NONE',  ( -0.9902903945359624593, -0.1390141521205945918, 0.000000000000000000 ) ) ;
#6306 = VECTOR ( 'NONE', #16096, 1000.000000000000341 ) ;
#6307 = CARTESIAN_POINT ( 'NONE',  ( 41.02212542604613077, 44.79787735033405482, 283.5832628385307999 ) ) ;
#6308 = ADVANCED_FACE ( 'NONE', ( #16044 ), #5003, .T. ) ;
#6309 = DIRECTION ( 'NONE',  ( 1.000000000000000000, 0.000000000000000000, 0.000000000000000000 ) ) ;
#6310 = CARTESIAN_POINT ( 'NONE',  ( -109.5721339228237667, 31.03941509555038181, 14.88498244535621851 ) ) ;
#6311 = FACE_OUTER_BOUND ( 'NONE', #18792, .T. ) ;
#6312 = VECTOR ( 'NONE', #2478, 1000.000000000000114 ) ;
#6313 = CARTESIAN_POINT ( 'NONE',  ( 150.0000000000000284, 1.836970198721029747E-14, -10.00000000000000178 ) ) ;
#6314 = FACE_OUTER_BOUND ( 'NONE', #15633, .T. ) ;
#6315 = CARTESIAN_POINT ( 'NONE',  ( 133.1515905083523705, -69.19806146150529003, 32.10257561466540466 ) ) ;
#6316 = CARTESIAN_POINT ( 'NONE',  ( 134.6712220124679789, -73.31159846691426196, 31.91396761802506177 ) ) ;
#6317 = VERTEX_POINT ( 'NONE', #14200 ) ;
#6318 = VERTEX_POINT ( 'NONE', #6540 ) ;
#6319 = AXIS2_PLACEMENT_3D ( 'NONE', #15251, #3193, #15460 ) ;
#6320 = CIRCLE ( 'NONE', #17749, 150.0000000000000284 ) ;
#6321 = ORIENTED_EDGE ( 'NONE', *, *, #7764, .F. ) ;
#6322 = EDGE_LOOP ( 'NONE', ( #4035, #10341, #17262, #11083 ) ) ;
#6323 = CARTESIAN_POINT ( 'NONE',  ( 67.08601213326539892, 40.32479851956841088, 132.4711112102474146 ) ) ;
#6324 = VERTEX_POINT ( 'NONE', #2031 ) ;
#6325 = DIRECTION ( 'NONE',  ( -0.8660254037844328234, -0.5000000000000101030, 0.000000000000000000 ) ) ;
#6326 = VECTOR ( 'NONE', #14293, 1000.000000000000114 ) ;
#6327 = CARTESIAN_POINT ( 'NONE',  ( -106.5749805965074728, -120.1845445602442624, 40.00000000000000000 ) ) ;
#6328 = CARTESIAN_POINT ( 'NONE',  ( 85.53020504959901871, -140.9188050298377846, 49.99999999999999289 ) ) ;
#6329 = LINE ( 'NONE', #9589, #2212 ) ;
#6330 = VERTEX_POINT ( 'NONE', #6438 ) ;
#6331 = CARTESIAN_POINT ( 'NONE',  ( 3.221721112346448201, 26.70531838198836283, 39.88498244535543336 ) ) ;
#6332 = DIRECTION ( 'NONE',  ( -0.000000000000000000, -0.000000000000000000, 1.000000000000000000 ) ) ;
#6333 = ORIENTED_EDGE ( 'NONE', *, *, #6968, .F. ) ;
#6334 = CARTESIAN_POINT ( 'NONE',  ( 30.05702882063027914, 50.41613078340812848, 248.9926560891072143 ) ) ;
#6336 = CIRCLE ( 'NONE', #10552, 112.8770930172170637 ) ;
#6335 = DIRECTION ( 'NONE',  ( 0.9394263059140722794, -0.3427509529624098161, 0.000000000000000000 ) ) ;
#6337 = CARTESIAN_POINT ( 'NONE',  ( -2.647132857508548209, -114.6332882433608376, 14.88498244535546888 ) ) ;
#6338 = CARTESIAN_POINT ( 'NONE',  ( 134.7188131032333445, -72.93593548660993520, 40.00000000000000711 ) ) ;
#6339 = VECTOR ( 'NONE', #19204, 1000.000000000000000 ) ;
#6340 = CARTESIAN_POINT ( 'NONE',  ( 0.000000000000000000, 0.000000000000000000, 49.99999999999999289 ) ) ;
#6341 = CARTESIAN_POINT ( 'NONE',  ( -15.91767397667354800, 164.0736214083062805, 49.99999999999999289 ) ) ;
#6342 = EDGE_LOOP ( 'NONE', ( #12963, #9955, #16291, #863 ) ) ;
#6343 = DIRECTION ( 'NONE',  ( -0.000000000000000000, -0.000000000000000000, 1.000000000000000000 ) ) ;
#6344 = CIRCLE ( 'NONE', #6015, 7.500000000000007994 ) ;
#6345 = EDGE_LOOP ( 'NONE', ( #2704, #2654, #10491, #575 ) ) ;
#6346 = VERTEX_POINT ( 'NONE', #285 ) ;
#6347 = LINE ( 'NONE', #12566, #7941 ) ;
#6348 = VERTEX_POINT ( 'NONE', #12761 ) ;
#6349 = CARTESIAN_POINT ( 'NONE',  ( -131.3857632021294535, 62.10379777574404869, -28.86798393970800092 ) ) ;
#6350 = CYLINDRICAL_SURFACE ( 'NONE', #9266, 112.8770930172170068 ) ;
#6351 = ORIENTED_EDGE ( 'NONE', *, *, #5742, .F. ) ;
#6352 = VECTOR ( 'NONE', #335, 1000.000000000000000 ) ;
#6353 = CARTESIAN_POINT ( 'NONE',  ( 83.25760956673217095, -124.7743995867201363, 2.742699998077471335 ) ) ;
#6354 = DIRECTION ( 'NONE',  ( 0.000000000000000000, 0.000000000000000000, 1.000000000000000000 ) ) ;
#6355 = EDGE_CURVE ( 'NONE', #20199, #10313, #19216, .T. ) ;
#6356 = VECTOR ( 'NONE', #19590, 1000.000000000000114 ) ;
#6357 = CARTESIAN_POINT ( 'NONE',  ( 114.2960429025576587, -28.68569479505797659, 14.88498244535465354 ) ) ;
#6358 = DIRECTION ( 'NONE',  ( -0.1390141521205912334, 0.9902903945359629034, 0.000000000000000000 ) ) ;
#6359 = EDGE_LOOP ( 'NONE', ( #19910, #10821, #5807, #17650 ) ) ;
#6360 = DIRECTION ( 'NONE',  ( 0.6427876096865379196, 0.7660444431189792347, 0.000000000000000000 ) ) ;
#6361 = DIRECTION ( 'NONE',  ( 0.9511061040868794558, 0.3088643371590157338, 0.000000000000000000 ) ) ;
#6362 = EDGE_CURVE ( 'NONE', #5578, #65, #14404, .T. ) ;
#6363 = DIRECTION ( 'NONE',  ( 0.000000000000000000, 0.000000000000000000, 1.000000000000000000 ) ) ;
#6364 = CARTESIAN_POINT ( 'NONE',  ( 82.65886493344478936, -125.1699850288369191, 35.14462631893170652 ) ) ;
#6365 = EDGE_LOOP ( 'NONE', ( #18082, #10976, #18465, #16950 ) ) ;
#6366 = EDGE_CURVE ( 'NONE', #10035, #19638, #19316, .T. ) ;
#6367 = CARTESIAN_POINT ( 'NONE',  ( -85.53020504959707182, -140.9188050298390067, 60.00000000000000000 ) ) ;
#6368 = CARTESIAN_POINT ( 'NONE',  ( -71.24814492356442486, 131.9990795557087893, 14.95622185591408027 ) ) ;
#6369 = ADVANCED_FACE ( 'NONE', ( #11526 ), #12956, .F. ) ;
#6370 = ORIENTED_EDGE ( 'NONE', *, *, #7341, .F. ) ;
#6371 = AXIS2_PLACEMENT_3D ( 'NONE', #12886, #8284, #9819 ) ;
#6372 = ORIENTED_EDGE ( 'NONE', *, *, #19988, .T. ) ;
#6373 = EDGE_CURVE ( 'NONE', #937, #9274, #15840, .T. ) ;
#6374 = EDGE_LOOP ( 'NONE', ( #1516, #12435, #651, #7838 ) ) ;
#6375 = ORIENTED_EDGE ( 'NONE', *, *, #16547, .T. ) ;
#6376 = LINE ( 'NONE', #1560, #7174 ) ;
#6377 = DIRECTION ( 'NONE',  ( -1.000000000000000000, 0.000000000000000000, 6.969309079188926949E-15 ) ) ;
#6378 = ORIENTED_EDGE ( 'NONE', *, *, #1111, .F. ) ;
#6379 = VECTOR ( 'NONE', #7269, 1000.000000000000000 ) ;
#6380 = DIRECTION ( 'NONE',  ( 0.4693298356057531984, -0.8830229359480288309, 0.000000000000000000 ) ) ;
#6381 = DIRECTION ( 'NONE',  ( 0.000000000000000000, 0.000000000000000000, 1.000000000000000000 ) ) ;
#6382 = LINE ( 'NONE', #10964, #7999 ) ;
#6383 = EDGE_CURVE ( 'NONE', #11666, #20199, #15942, .T. ) ;
#6384 = CARTESIAN_POINT ( 'NONE',  ( -101.9549241234480803, -127.6987521375408363, 38.34482911501410030 ) ) ;
#6385 = CIRCLE ( 'NONE', #16822, 7.500000000000002665 ) ;
#6386 = DIRECTION ( 'NONE',  ( 0.000000000000000000, 0.000000000000000000, 1.000000000000000000 ) ) ;
#6387 = CARTESIAN_POINT ( 'NONE',  ( -96.48501399889541119, -114.8592206156971542, -9.502595028825394863 ) ) ;
#6388 =( BOUNDED_SURFACE ( )  B_SPLINE_SURFACE ( 3, 2, ( 
 ( #15267, #19769, #6074 ),
 ( #16514, #1253, #11881 ),
 ( #4120, #10350, #16608 ),
 ( #2595, #8824, #15064 ),
 ( #5766, #11982, #17335 ),
 ( #4531, #228, #6287 ),
 ( #12399, #15477, #6182 ),
 ( #6487, #20181, #15692 ),
 ( #3207, #1673, #4956 ),
 ( #18662, #4638, #6384 ),
 ( #7899, #11070, #9445 ),
 ( #14044, #9233, #1462 ),
 ( #3004, #4850, #10863 ),
 ( #12600, #17118, #17017 ),
 ( #3311, #11173, #12498 ),
 ( #12706, #14145, #10764 ),
 ( #7691, #132, #18864 ),
 ( #13936, #3105, #10966 ),
 ( #9336, #15582, #1568 ),
 ( #9546, #7803, #4743 ),
 ( #33, #15786, #1771 ),
 ( #18763, #8003, #17227 ),
 ( #14249, #18969, #15229 ),
 ( #16775, #20146, #2765 ),
 ( #10825, #19734, #8988 ),
 ( #16679, #16875, #15442 ),
 ( #13799, #4393, #19833 ),
 ( #5831, #9092, #8890 ),
 ( #1214, #13484, #5942 ),
 ( #12156, #15035, #4495 ),
 ( #7456, #7262, #9197 ),
 ( #20044, #10619, #12050 ) ),
 .UNSPECIFIED., .F., .F., .F. ) 
 B_SPLINE_SURFACE_WITH_KNOTS ( ( 4, 2, 2, 2, 2, 2, 2, 2, 2, 2, 2, 2, 2, 2, 2, 4 ),
 ( 3, 3 ),
 ( 0.02531008572351745728, 0.02976618726483494168, 0.03422228880615242608, 0.03645033957681116654, 0.03867839034746990701, 0.04313449188878738794, 0.04424851727411675817, 0.04536254265944612840, 0.04759059343010486887, 0.04981864420076360933, 0.05093266958609297956, 0.05204669497142234980, 0.05650279651273983073, 0.05761682189806920096, 0.05873084728339857119, 0.06095889805405731859 ),
 ( 0.000000000000000000, 1.000000000000000000 ),
 .UNSPECIFIED. ) 
 GEOMETRIC_REPRESENTATION_ITEM ( )  RATIONAL_B_SPLINE_SURFACE ( (
 ( 1.000000000000000000, 0.7071067811865477948, 1.000000000000000000),
 ( 1.000000000000000000, 0.6938858163893895092, 1.000000000000000000),
 ( 1.000000000000000000, 0.6806631601997592540, 1.000000000000000000),
 ( 1.000000000000000000, 0.6542661407889984737, 1.000000000000000000),
 ( 1.000000000000000000, 0.6410910482671290378, 1.000000000000000000),
 ( 1.000000000000000000, 0.6214215355381913497, 1.000000000000000000),
 ( 1.000000000000000000, 0.6148567640636197762, 1.000000000000000000),
 ( 1.000000000000000000, 0.6019746658715365850, 1.000000000000000000),
 ( 1.000000000000000000, 0.5956402134854033026, 1.000000000000000000),
 ( 1.000000000000000000, 0.5769855966605448305, 1.000000000000000000),
 ( 1.000000000000000000, 0.5650096313357982902, 1.000000000000000000),
 ( 1.000000000000000000, 0.5507648555195425732, 1.000000000000000000),
 ( 1.000000000000000000, 0.5479490128870788679, 1.000000000000000000),
 ( 1.000000000000000000, 0.5424554856653597268, 1.000000000000000000),
 ( 1.000000000000000000, 0.5397704441657605878, 1.000000000000000000),
 ( 1.000000000000000000, 0.5319045985430522760, 1.000000000000000000),
 ( 1.000000000000000000, 0.5269125948469715048, 1.000000000000000000),
 ( 1.000000000000000000, 0.5174644824776444274, 1.000000000000000000),
 ( 1.000000000000000000, 0.5130081457584507731, 1.000000000000000000),
 ( 1.000000000000000000, 0.5067628861632463844, 1.000000000000000000),
 ( 1.000000000000000000, 0.5047490957320780458, 1.000000000000000000),
 ( 1.000000000000000000, 0.5009263418717803118, 1.000000000000000000),
 ( 1.000000000000000000, 0.4991119735066952279, 1.000000000000000000),
 ( 1.000000000000000000, 0.4905251103113591471, 1.000000000000000000),
 ( 1.000000000000000000, 0.4851887169573420033, 1.000000000000000000),
 ( 1.000000000000000000, 0.4806071066593465835, 1.000000000000000000),
 ( 1.000000000000000000, 0.4797938356042399377, 1.000000000000000000),
 ( 1.000000000000000000, 0.4784048377100982297, 1.000000000000000000),
 ( 1.000000000000000000, 0.4778282137465386104, 1.000000000000000000),
 ( 1.000000000000000000, 0.4764456491723553233, 1.000000000000000000),
 ( 1.000000000000000000, 0.4759864261380953310, 1.000000000000000000),
 ( 1.000000000000000000, 0.4759858191164941243, 1.000000000000000000) ) ) 
 REPRESENTATION_ITEM ( '' )  SURFACE ( )  );
#6389 = DIRECTION ( 'NONE',  ( 0.000000000000000000, 0.000000000000000000, 1.000000000000000000 ) ) ;
#6390 = DIRECTION ( 'NONE',  ( 0.7881095627315598540, 0.6155349844899715706, 0.000000000000000000 ) ) ;
#6391 = DIRECTION ( 'NONE',  ( 0.000000000000000000, 0.000000000000000000, 1.000000000000000000 ) ) ;
#6392 = CARTESIAN_POINT ( 'NONE',  ( -133.6156149914909008, -80.24737158797381653, 37.64197558898200668 ) ) ;
#6393 = ORIENTED_EDGE ( 'NONE', *, *, #13851, .F. ) ;
#6394 = EDGE_CURVE ( 'NONE', #17239, #18566, #17550, .T. ) ;
#6395 = FACE_OUTER_BOUND ( 'NONE', #10081, .T. ) ;
#6396 = ADVANCED_FACE ( 'NONE', ( #3561 ), #9895, .F. ) ;
#6397 = AXIS2_PLACEMENT_3D ( 'NONE', #1739, #11042, #9518 ) ;
#6398 = EDGE_CURVE ( 'NONE', #5054, #1479, #14601, .T. ) ;
#6399 = ORIENTED_EDGE ( 'NONE', *, *, #17137, .T. ) ;
#6400 = ORIENTED_EDGE ( 'NONE', *, *, #3384, .F. ) ;
#6401 = ORIENTED_EDGE ( 'NONE', *, *, #12375, .T. ) ;
#6402 = ADVANCED_FACE ( 'NONE', ( #13347 ), #8557, .F. ) ;
#6403 = CARTESIAN_POINT ( 'NONE',  ( -39.84224160888947353, -67.36461649554519227, 248.9926560891072143 ) ) ;
#6404 = CARTESIAN_POINT ( 'NONE',  ( 19.63382932406824466, 18.38657833536341357, 14.88498244535531256 ) ) ;
#6405 = VECTOR ( 'NONE', #12468, 1000.000000000000114 ) ;
#6406 = CARTESIAN_POINT ( 'NONE',  ( 181.0783081749256951, -199.9999999999999716, 0.000000000000000000 ) ) ;
#6407 = DIRECTION ( 'NONE',  ( -0.7071067811865516806, 8.659560562354883554E-17, -0.7071067811865434649 ) ) ;
#6408 = CARTESIAN_POINT ( 'NONE',  ( -24.73834469112680523, -10.56256686379325593, 39.88498244535562520 ) ) ;
#6409 = PLANE ( 'NONE',  #10104 ) ;
#6410 = CARTESIAN_POINT ( 'NONE',  ( 97.50000000000000000, -133.9542832461881119, 30.48586822279154873 ) ) ;
#6411 = DIRECTION ( 'NONE',  ( -0.000000000000000000, -0.000000000000000000, 1.000000000000000000 ) ) ;
#6412 = ORIENTED_EDGE ( 'NONE', *, *, #4503, .T. ) ;
#6413 = ADVANCED_FACE ( 'NONE', ( #19798 ), #2329, .F. ) ;
#6414 = CARTESIAN_POINT ( 'NONE',  ( 28.06584155524102187, -53.86996498385662591, 283.5832628385307999 ) ) ;
#6415 = EDGE_CURVE ( 'NONE', #13679, #6070, #18168, .T. ) ;
#6416 = CARTESIAN_POINT ( 'NONE',  ( -110.0000000000000142, 275.0000000000000000, -29.99999999999998224 ) ) ;
#6418 = EDGE_CURVE ( 'NONE', #13999, #18902, #688, .T. ) ;
#6417 = CIRCLE ( 'NONE', #8372, 15.91767397667354267 ) ;
#6419 = VERTEX_POINT ( 'NONE', #13548 ) ;
#6420 = ORIENTED_EDGE ( 'NONE', *, *, #16379, .T. ) ;
#6421 = B_SPLINE_CURVE_WITH_KNOTS ( 'NONE', 3,
 ( #3565, #8261, #3953, #16252, #5303, #11532, #2233, #588, #3665, #494, #16346, #7133 ),
 .UNSPECIFIED., .F., .F.,
 ( 4, 2, 2, 2, 2, 4 ),
 ( 0.000000000000000000, 0.004378549521624888058, 0.008757099043249776116, 0.01094637380406223229, 0.01313564856487468846, 0.01751419808649958346 ),
 .UNSPECIFIED. ) ;
#6422 = ORIENTED_EDGE ( 'NONE', *, *, #14917, .T. ) ;
#6423 = EDGE_CURVE ( 'NONE', #13125, #9217, #3949, .T. ) ;
#6424 = ORIENTED_EDGE ( 'NONE', *, *, #15760, .F. ) ;
#6425 = DIRECTION ( 'NONE',  ( 0.000000000000000000, 0.000000000000000000, 1.000000000000000000 ) ) ;
#6426 = ORIENTED_EDGE ( 'NONE', *, *, #14342, .F. ) ;
#6427 = DIRECTION ( 'NONE',  ( 0.9396926207859068736, 0.3420201433256725987, 0.000000000000000000 ) ) ;
#6428 = CARTESIAN_POINT ( 'NONE',  ( 7.948651060879040386, -60.22029172860440127, 283.5832628385307999 ) ) ;
#6429 = DIRECTION ( 'NONE',  ( 0.000000000000000000, 0.000000000000000000, 1.000000000000000000 ) ) ;
#6430 = DIRECTION ( 'NONE',  ( 0.000000000000000000, 0.000000000000000000, 1.000000000000000000 ) ) ;
#6431 = DIRECTION ( 'NONE',  ( 0.000000000000000000, 0.000000000000000000, 1.000000000000000000 ) ) ;
#6432 = ORIENTED_EDGE ( 'NONE', *, *, #16130, .T. ) ;
#6433 = DIRECTION ( 'NONE',  ( -0.000000000000000000, 0.000000000000000000, 1.000000000000000000 ) ) ;
#6434 = DIRECTION ( 'NONE',  ( -0.000000000000000000, -0.000000000000000000, -1.000000000000000000 ) ) ;
#6435 = AXIS2_PLACEMENT_3D ( 'NONE', #17070, #13783, #15427 ) ;
#6436 = ORIENTED_EDGE ( 'NONE', *, *, #9613, .T. ) ;
#6437 = CIRCLE ( 'NONE', #8693, 60.74260934110282051 ) ;
#6438 = CARTESIAN_POINT ( 'NONE',  ( 7.500000000000001776, 60.00000000000000000, -100.0000000000000000 ) ) ;
#6439 = CARTESIAN_POINT ( 'NONE',  ( -8.402595070144922573, -117.5408478153264298, 39.88498244535551862 ) ) ;
#6440 = FACE_OUTER_BOUND ( 'NONE', #16482, .T. ) ;
#6441 = AXIS2_PLACEMENT_3D ( 'NONE', #2235, #18079, #13155 ) ;
#6442 = CARTESIAN_POINT ( 'NONE',  ( 0.000000000000000000, 0.000000000000000000, 60.00000000000000000 ) ) ;
#6443 = DIRECTION ( 'NONE',  ( 1.000000000000000000, 0.000000000000000000, 0.000000000000000000 ) ) ;
#6444 = CARTESIAN_POINT ( 'NONE',  ( 88.72241907111769876, -120.9490000788567130, 45.32939563125253102 ) ) ;
#6445 = ORIENTED_EDGE ( 'NONE', *, *, #6884, .F. ) ;
#6446 = DIRECTION ( 'NONE',  ( -0.7660444431189726844, -0.6427876096865456912, 0.000000000000000000 ) ) ;
#6447 = VERTEX_POINT ( 'NONE', #19696 ) ;
#6448 = AXIS2_PLACEMENT_3D ( 'NONE', #19999, #1173, #20206 ) ;
#6449 = EDGE_CURVE ( 'NONE', #2619, #9376, #10029, .T. ) ;
#6450 = EDGE_LOOP ( 'NONE', ( #16473, #789 ) ) ;
#6451 = CARTESIAN_POINT ( 'NONE',  ( 7.950000000000000178, 1.102182119232617911E-15, -9.000000000000001776 ) ) ;
#6452 = VERTEX_POINT ( 'NONE', #8458 ) ;
#6453 = DIRECTION ( 'NONE',  ( 1.000000000000000000, 0.000000000000000000, 0.000000000000000000 ) ) ;
#6454 = VECTOR ( 'NONE', #8587, 1000.000000000000000 ) ;
#6455 = DIRECTION ( 'NONE',  ( -0.9396926207859057634, -0.3420201433256757073, 0.000000000000000000 ) ) ;
#6456 = VECTOR ( 'NONE', #10266, 1000.000000000000000 ) ;
#6457 = ORIENTED_EDGE ( 'NONE', *, *, #17062, .F. ) ;
#6458 = CARTESIAN_POINT ( 'NONE',  ( 36.66871011346380982, 45.84586732611875703, 132.4711112102474146 ) ) ;
#6459 = FACE_OUTER_BOUND ( 'NONE', #13648, .T. ) ;
#6460 = DIRECTION ( 'NONE',  ( 0.3420201433256568335, 0.9396926207859126468, 0.000000000000000000 ) ) ;
#6461 = PLANE ( 'NONE',  #10921 ) ;
#6462 = VERTEX_POINT ( 'NONE', #5795 ) ;
#6463 = DIRECTION ( 'NONE',  ( 0.000000000000000000, 0.000000000000000000, 1.000000000000000000 ) ) ;
#6464 = CARTESIAN_POINT ( 'NONE',  ( 21.36933070621763164, -54.67896814532648619, 111.4180192758973362 ) ) ;
#6465 = DIRECTION ( 'NONE',  ( 1.000000000000000000, 0.000000000000000000, 0.000000000000000000 ) ) ;
#6466 = CARTESIAN_POINT ( 'NONE',  ( 62.91752772691707207, 0.000000000000000000, 83.57543755549745867 ) ) ;
#6467 = ORIENTED_EDGE ( 'NONE', *, *, #12717, .T. ) ;
#6468 = AXIS2_PLACEMENT_3D ( 'NONE', #7753, #15846, #12865 ) ;
#6469 = LINE ( 'NONE', #14536, #2244 ) ;
#6470 = CARTESIAN_POINT ( 'NONE',  ( -72.24243551186484069, 131.4596132301078057, -8.327469122224886888 ) ) ;
#6471 = VECTOR ( 'NONE', #16120, 1000.000000000000000 ) ;
#6472 = ORIENTED_EDGE ( 'NONE', *, *, #5756, .F. ) ;
#6473 = ADVANCED_FACE ( 'NONE', ( #14699 ), #10286, .T. ) ;
#6474 = ORIENTED_EDGE ( 'NONE', *, *, #11766, .F. ) ;
#6475 = ORIENTED_EDGE ( 'NONE', *, *, #13910, .F. ) ;
#6476 = CARTESIAN_POINT ( 'NONE',  ( 0.000000000000000000, 0.000000000000000000, 0.000000000000000000 ) ) ;
#6477 = ORIENTED_EDGE ( 'NONE', *, *, #8045, .F. ) ;
#6478 = DIRECTION ( 'NONE',  ( -0.4693298356057531429, 0.8830229359480288309, 0.000000000000000000 ) ) ;
#6479 = CARTESIAN_POINT ( 'NONE',  ( -145.8049199971885344, 35.51790619049093323, 22.99421396143800678 ) ) ;
#6480 = ORIENTED_EDGE ( 'NONE', *, *, #12258, .T. ) ;
#6481 = CARTESIAN_POINT ( 'NONE',  ( 0.000000000000000000, 164.0736214083062805, 39.99999999999999289 ) ) ;
#6482 = DIRECTION ( 'NONE',  ( 0.4974449862757516216, 0.000000000000000000, 0.8674955248467378643 ) ) ;
#6483 = DIRECTION ( 'NONE',  ( 1.000000000000000000, 0.000000000000000000, 0.000000000000000000 ) ) ;
#6484 = AXIS2_PLACEMENT_3D ( 'NONE', #2123, #14693, #680 ) ;
#6485 = VECTOR ( 'NONE', #18378, 1000.000000000000000 ) ;
#6486 = EDGE_CURVE ( 'NONE', #3220, #12611, #14890, .T. ) ;
#6487 = CARTESIAN_POINT ( 'NONE',  ( -92.40373333587341165, -118.1608478542227942, 47.90302656145166083 ) ) ;
#6488 = CARTESIAN_POINT ( 'NONE',  ( 60.47951622432751151, 49.67518383744852883, 110.7293897666001214 ) ) ;
#6489 = DIRECTION ( 'NONE',  ( -0.000000000000000000, -0.000000000000000000, 1.000000000000000000 ) ) ;
#6490 = DIRECTION ( 'NONE',  ( 1.000000000000000000, 0.000000000000000000, 0.000000000000000000 ) ) ;
#6491 = DIRECTION ( 'NONE',  ( -0.9749279121818226201, -0.2225209339563185285, 0.000000000000000000 ) ) ;
#6492 = DIRECTION ( 'NONE',  ( -6.982962677686266711E-15, 0.000000000000000000, -1.000000000000000000 ) ) ;
#6493 = CARTESIAN_POINT ( 'NONE',  ( -134.4267602304430795, -75.13220794377609479, 34.41794545084487567 ) ) ;
#6494 = VERTEX_POINT ( 'NONE', #1070 ) ;
#6495 = CYLINDRICAL_SURFACE ( 'NONE', #19989, 7.500000000000000000 ) ;
#6496 = AXIS2_PLACEMENT_3D ( 'NONE', #2149, #10113, #1837 ) ;
#6497 = VECTOR ( 'NONE', #8722, 1000.000000000000000 ) ;
#6498 = EDGE_CURVE ( 'NONE', #1969, #3773, #13148, .T. ) ;
#6499 = AXIS2_PLACEMENT_3D ( 'NONE', #18955, #17620, #14439 ) ;
#6500 = VERTEX_POINT ( 'NONE', #17879 ) ;
#6501 = ORIENTED_EDGE ( 'NONE', *, *, #9616, .F. ) ;
#6502 = ORIENTED_EDGE ( 'NONE', *, *, #5861, .F. ) ;
#6503 = CARTESIAN_POINT ( 'NONE',  ( -142.3282607959048960, -17.64421488672613947, -8.419224594817324103 ) ) ;
#6504 = LINE ( 'NONE', #4659, #9941 ) ;
#6505 = ADVANCED_FACE ( 'NONE', ( #3851 ), #782, .T. ) ;
#6506 = CARTESIAN_POINT ( 'NONE',  ( 0.000000000000000000, 0.000000000000000000, 39.99999999999999289 ) ) ;
#6507 = AXIS2_PLACEMENT_3D ( 'NONE', #2644, #3963, #7334 ) ;
#6508 = DIRECTION ( 'NONE',  ( 0.4338837391175526248, 0.9009688679024218105, -0.000000000000000000 ) ) ;
#6509 = CARTESIAN_POINT ( 'NONE',  ( 0.000000000000000000, 0.000000000000000000, 132.4711112102474146 ) ) ;
#6510 = VECTOR ( 'NONE', #1625, 1000.000000000000227 ) ;
#6511 = ADVANCED_FACE ( 'NONE', ( #10377 ), #11714, .F. ) ;
#6512 = DIRECTION ( 'NONE',  ( 0.7660444431189792347, -0.6427876096865379196, -0.000000000000000000 ) ) ;
#6513 = AXIS2_PLACEMENT_3D ( 'NONE', #8328, #14473, #255 ) ;
#6514 = CARTESIAN_POINT ( 'NONE',  ( -67.08601213326564050, -40.32479851956793482, 248.9926560891072143 ) ) ;
#6515 = CARTESIAN_POINT ( 'NONE',  ( -60.00000000000000000, -2.094888803305880013E-13, -115.0000000000000000 ) ) ;
#6516 = DIRECTION ( 'NONE',  ( -0.000000000000000000, -0.000000000000000000, 1.000000000000000000 ) ) ;
#6517 = DIRECTION ( 'NONE',  ( 0.03505990758545895342, 0.9993852124581886764, 0.000000000000000000 ) ) ;
#6518 = ORIENTED_EDGE ( 'NONE', *, *, #4898, .F. ) ;
#6519 = CARTESIAN_POINT ( 'NONE',  ( 133.0788080491229550, -69.33756331726938527, 32.62557982921207866 ) ) ;
#6520 = CARTESIAN_POINT ( 'NONE',  ( 134.6433994324794412, -73.52870175801844255, 32.36516242777680219 ) ) ;
#6521 = ORIENTED_EDGE ( 'NONE', *, *, #17186, .T. ) ;
#6522 = EDGE_LOOP ( 'NONE', ( #12615, #11801, #4797, #2709 ) ) ;
#6523 = EDGE_CURVE ( 'NONE', #2113, #98, #18073, .T. ) ;
#6524 = ORIENTED_EDGE ( 'NONE', *, *, #8233, .T. ) ;
#6525 = AXIS2_PLACEMENT_3D ( 'NONE', #3433, #17756, #4977 ) ;
#6526 = CIRCLE ( 'NONE', #13336, 60.74260934110282051 ) ;
#6527 = ORIENTED_EDGE ( 'NONE', *, *, #11158, .T. ) ;
#6528 = CARTESIAN_POINT ( 'NONE',  ( 51.77076963420846312, -31.77187437101485656, 283.5832628385307999 ) ) ;
#6529 = VERTEX_POINT ( 'NONE', #16640 ) ;
#6530 = LINE ( 'NONE', #1614, #7709 ) ;
#6531 = DIRECTION ( 'NONE',  ( 1.000000000000000000, 0.000000000000000000, 0.000000000000000000 ) ) ;
#6532 = CARTESIAN_POINT ( 'NONE',  ( -31.77187437101503775, -51.77076963420834943, 283.5832628385307999 ) ) ;
#6533 = DIRECTION ( 'NONE',  ( -0.4338837391175523472, -0.9009688679024219216, 0.000000000000000000 ) ) ;
#6534 = ORIENTED_EDGE ( 'NONE', *, *, #11874, .F. ) ;
#6535 = EDGE_CURVE ( 'NONE', #7331, #20085, #2195, .T. ) ;
#6536 = DIRECTION ( 'NONE',  ( 0.8186676071302493307, 0.5742676632334713371, 0.000000000000000000 ) ) ;
#6537 = DIRECTION ( 'NONE',  ( 0.000000000000000000, 0.000000000000000000, 1.000000000000000000 ) ) ;
#6538 = EDGE_CURVE ( 'NONE', #18899, #12185, #8752, .T. ) ;
#6539 = ORIENTED_EDGE ( 'NONE', *, *, #19103, .T. ) ;
#6540 = CARTESIAN_POINT ( 'NONE',  ( -13.12726406102078336, -59.30716253403180360, 293.5832628385307999 ) ) ;
#6541 = CYLINDRICAL_SURFACE ( 'NONE', #6838, 62.91752772691707207 ) ;
#6542 = FACE_BOUND ( 'NONE', #11056, .T. ) ;
#6543 = CIRCLE ( 'NONE', #6507, 10.00000000000000888 ) ;
#6544 = AXIS2_PLACEMENT_3D ( 'NONE', #8848, #13650, #2719 ) ;
#6545 = DIRECTION ( 'NONE',  ( -0.7660444431189813441, 0.6427876096865353661, 0.000000000000000000 ) ) ;
#6546 = CARTESIAN_POINT ( 'NONE',  ( 0.000000000000000000, 0.000000000000000000, 293.5832628385307999 ) ) ;
#6547 = PLANE ( 'NONE',  #4804 ) ;
#6548 = ORIENTED_EDGE ( 'NONE', *, *, #12349, .F. ) ;
#6549 = CARTESIAN_POINT ( 'NONE',  ( 76.92888220842486646, -14.39940464655733976, 248.9926560891072143 ) ) ;
#6550 = EDGE_CURVE ( 'NONE', #7508, #15218, #13692, .T. ) ;
#6551 = VERTEX_POINT ( 'NONE', #10578 ) ;
#6552 = ORIENTED_EDGE ( 'NONE', *, *, #15997, .T. ) ;
#6553 = DIRECTION ( 'NONE',  ( -1.000000000000000000, 0.000000000000000000, 0.000000000000000000 ) ) ;
#6554 = ORIENTED_EDGE ( 'NONE', *, *, #16422, .F. ) ;
#6555 = AXIS2_PLACEMENT_3D ( 'NONE', #17638, #3612, #9842 ) ;
#6556 = CYLINDRICAL_SURFACE ( 'NONE', #16010, 15.91767397667355510 ) ;
#6557 = DIRECTION ( 'NONE',  ( 0.000000000000000000, 0.000000000000000000, 1.000000000000000000 ) ) ;
#6558 = VERTEX_POINT ( 'NONE', #12221 ) ;
#6559 = EDGE_CURVE ( 'NONE', #6529, #19079, #1288, .T. ) ;
#6560 = LINE ( 'NONE', #13072, #4766 ) ;
#6561 = DIRECTION ( 'NONE',  ( 6.982962677686266711E-15, -0.000000000000000000, 1.000000000000000000 ) ) ;
#6562 = PLANE ( 'NONE',  #19959 ) ;
#6563 = DIRECTION ( 'NONE',  ( 0.000000000000000000, 0.000000000000000000, 1.000000000000000000 ) ) ;
#6564 = ADVANCED_FACE ( 'NONE', ( #5897 ), #18581, .F. ) ;
#6565 = CARTESIAN_POINT ( 'NONE',  ( 30.25670013172214468, 55.16472960512381718, 132.4711112102474146 ) ) ;
#6566 = DIRECTION ( 'NONE',  ( -1.000000000000000000, -0.000000000000000000, -0.000000000000000000 ) ) ;
#6567 = ORIENTED_EDGE ( 'NONE', *, *, #6538, .T. ) ;
#6568 = CARTESIAN_POINT ( 'NONE',  ( -97.95177330934026827, 59.60912842347561025, 14.88498244535613502 ) ) ;
#6569 = LINE ( 'NONE', #10946, #11966 ) ;
#6570 = CARTESIAN_POINT ( 'NONE',  ( 7.950000000000000178, 5.196152422706627583, 9.000000000000001776 ) ) ;
#6571 = CIRCLE ( 'NONE', #7863, 150.0000000000000284 ) ;
#6572 = CARTESIAN_POINT ( 'NONE',  ( 0.000000000000000000, 0.000000000000000000, 60.00000000000000000 ) ) ;
#6573 = EDGE_LOOP ( 'NONE', ( #673, #1068, #223, #1503 ) ) ;
#6574 = CARTESIAN_POINT ( 'NONE',  ( 0.000000000000000000, 0.000000000000000000, 293.5832628385307999 ) ) ;
#6575 = CARTESIAN_POINT ( 'NONE',  ( 0.000000000000000000, 0.000000000000000000, 49.99999999999999289 ) ) ;
#6576 = ORIENTED_EDGE ( 'NONE', *, *, #13406, .F. ) ;
#6577 = ORIENTED_EDGE ( 'NONE', *, *, #15894, .F. ) ;
#6578 = ORIENTED_EDGE ( 'NONE', *, *, #11221, .F. ) ;
#6579 = APPLICATION_PROTOCOL_DEFINITION ( 'draft international standard', 'automotive_design', 1998, #17313 ) ;
#6580 = ORIENTED_EDGE ( 'NONE', *, *, #4118, .F. ) ;
#6581 = LINE ( 'NONE', #10756, #16967 ) ;
#6582 = AXIS2_PLACEMENT_3D ( 'NONE', #10528, #15344, #6055 ) ;
#6583 = CARTESIAN_POINT ( 'NONE',  ( -149.9377538849844882, 4.462546922558185081, 7.303857415559938282 ) ) ;
#6584 = EDGE_LOOP ( 'NONE', ( #15552, #8121, #10567, #455 ) ) ;
#6585 = AXIS2_PLACEMENT_3D ( 'NONE', #5376, #14681, #6912 ) ;
#6586 = CARTESIAN_POINT ( 'NONE',  ( 36.66871011346380982, 45.84586732611875703, 110.7293897666001214 ) ) ;
#6587 = CARTESIAN_POINT ( 'NONE',  ( 73.25972925305627825, -27.53920554013664912, 248.9926560891072143 ) ) ;
#6588 = CARTESIAN_POINT ( 'NONE',  ( 131.6317334595287036, -71.92650142027842719, 44.25146303588275742 ) ) ;
#6589 = CARTESIAN_POINT ( 'NONE',  ( -13.12769224524071277, -59.30917539369501412, 283.5832628385307999 ) ) ;
#6590 = DIRECTION ( 'NONE',  ( 0.000000000000000000, 0.000000000000000000, -1.000000000000000000 ) ) ;
#6591 = EDGE_CURVE ( 'NONE', #15414, #16327, #9264, .T. ) ;
#6592 = CARTESIAN_POINT ( 'NONE',  ( 59.39925916207545242, 20.74471755083624203, 248.9926560891072143 ) ) ;
#6593 = CARTESIAN_POINT ( 'NONE',  ( 106.6880305650188205, 105.4403344747995988, 49.99999999999999289 ) ) ;
#6594 = CARTESIAN_POINT ( 'NONE',  ( -29.99999999999887379, 275.0000000000000000, 12.49999999999916511 ) ) ;
#6595 = ORIENTED_EDGE ( 'NONE', *, *, #17619, .T. ) ;
#6596 = AXIS2_PLACEMENT_3D ( 'NONE', #11352, #14220, #15863 ) ;
#6597 = CARTESIAN_POINT ( 'NONE',  ( -138.4582331060196623, 17.23264747863311896, -15.37944944523201585 ) ) ;
#6598 = B_SPLINE_CURVE_WITH_KNOTS ( 'NONE', 3,
 ( #1675, #15892, #14047, #7903, #14357, #6387, #17438, #12603, #1871, #15791, #8102, #8006, #230, #333, #19553, #8608, #928, #17830, #10050, #5542, #16394, #16299, #14750, #11672, #3902, #18120, #7078, #2186, #8410, #14842 ),
 .UNSPECIFIED., .F., .F.,
 ( 4, 2, 2, 2, 2, 2, 2, 2, 2, 2, 2, 2, 2, 2, 4 ),
 ( 0.000000000000000000, 0.002170930610089446579, 0.004341861220178893158, 0.008683722440357753355, 0.01085465305044718519, 0.01302558366053661876, 0.01519651427062605059, 0.01736744488071548242, 0.02170930610089434956, 0.02388023671098378140, 0.02605116732107320629, 0.02822209793116263465, 0.02930756323620734363, 0.03039302854125205608, 0.03473488976143088158 ),
 .UNSPECIFIED. ) ;
#6599 = ORIENTED_EDGE ( 'NONE', *, *, #5993, .T. ) ;
#6600 = ORIENTED_EDGE ( 'NONE', *, *, #13074, .T. ) ;
#6601 = ORIENTED_EDGE ( 'NONE', *, *, #6622, .F. ) ;
#6602 = CARTESIAN_POINT ( 'NONE',  ( 135.1060089022256818, -65.16414933467422088, 30.00000000000000000 ) ) ;
#6603 = CYLINDRICAL_SURFACE ( 'NONE', #9618, 17.50000000000001066 ) ;
#6604 = CARTESIAN_POINT ( 'NONE',  ( 0.7000608949449915741, 5.693982670708925831, 293.5832628385307999 ) ) ;
#6605 = CARTESIAN_POINT ( 'NONE',  ( -40.32479851956768613, 67.08601213326579682, 110.9660488491356887 ) ) ;
#6606 = EDGE_CURVE ( 'NONE', #4738, #11620, #16941, .T. ) ;
#6607 = ORIENTED_EDGE ( 'NONE', *, *, #3616, .T. ) ;
#6608 = LINE ( 'NONE', #156, #3882 ) ;
#6609 = LINE ( 'NONE', #16116, #7911 ) ;
#6610 = DIRECTION ( 'NONE',  ( 0.7660444431189858960, -0.6427876096865300370, 0.000000000000000000 ) ) ;
#6611 = VECTOR ( 'NONE', #13223, 1000.000000000000000 ) ;
#6612 = CARTESIAN_POINT ( 'NONE',  ( 1.396592535537253342E-14, 0.000000000000000000, 43.88498244535545467 ) ) ;
#6613 = CARTESIAN_POINT ( 'NONE',  ( 4.581103194069847007, -3.453261854572897693, 293.5832628385307999 ) ) ;
#6614 = ORIENTED_EDGE ( 'NONE', *, *, #16884, .T. ) ;
#6615 = DIRECTION ( 'NONE',  ( 0.000000000000000000, 0.000000000000000000, 1.000000000000000000 ) ) ;
#6616 = DIRECTION ( 'NONE',  ( 0.000000000000000000, 0.000000000000000000, -1.000000000000000000 ) ) ;
#6617 = ORIENTED_EDGE ( 'NONE', *, *, #19589, .F. ) ;
#6618 = EDGE_CURVE ( 'NONE', #8834, #818, #227, .T. ) ;
#6619 = ORIENTED_EDGE ( 'NONE', *, *, #12893, .T. ) ;
#6620 = ADVANCED_FACE ( 'NONE', ( #8948 ), #15507, .T. ) ;
#6621 = EDGE_LOOP ( 'NONE', ( #163, #5630, #8810, #12591 ) ) ;
#6622 = EDGE_CURVE ( 'NONE', #6500, #10158, #15608, .T. ) ;
#6623 = DIRECTION ( 'NONE',  ( -0.000000000000000000, -0.000000000000000000, 1.000000000000000000 ) ) ;
#6624 = AXIS2_PLACEMENT_3D ( 'NONE', #18562, #15701, #4546 ) ;
#6625 = AXIS2_PLACEMENT_3D ( 'NONE', #1027, #10332, #7273 ) ;
#6626 = VERTEX_POINT ( 'NONE', #4350 ) ;
#6627 = FACE_OUTER_BOUND ( 'NONE', #6208, .T. ) ;
#6628 = DIRECTION ( 'NONE',  ( 1.000000000000000000, 0.000000000000000000, -7.137148015447434001E-15 ) ) ;
#6629 = LINE ( 'NONE', #12444, #1440 ) ;
#6630 = DIRECTION ( 'NONE',  ( -1.000000000000000000, 0.000000000000000000, 0.000000000000000000 ) ) ;
#6631 = ORIENTED_EDGE ( 'NONE', *, *, #5121, .F. ) ;
#6632 = VECTOR ( 'NONE', #16377, 1000.000000000000000 ) ;
#6633 = CARTESIAN_POINT ( 'NONE',  ( 134.6444961603440902, -66.11310837778572136, 4.324214274277042414 ) ) ;
#6634 = CARTESIAN_POINT ( 'NONE',  ( 77.31114765718494652, -12.23146955673620795, 112.0427633081292385 ) ) ;
#6635 = EDGE_CURVE ( 'NONE', #1924, #19563, #5455, .T. ) ;
#6636 = ORIENTED_EDGE ( 'NONE', *, *, #9012, .T. ) ;
#6637 = CARTESIAN_POINT ( 'NONE',  ( -110.0000000000000142, 165.0000000000000000, -34.99999999999997868 ) ) ;
#6638 = CARTESIAN_POINT ( 'NONE',  ( -109.9999999999983515, 265.0000000000000000, 77.50000000000000000 ) ) ;
#6639 = CARTESIAN_POINT ( 'NONE',  ( 141.8714406926367815, -48.70825716237079916, 49.99999999999999289 ) ) ;
#6640 = VECTOR ( 'NONE', #20166, 1000.000000000000000 ) ;
#6641 = LINE ( 'NONE', #290, #12307 ) ;
#6642 = CYLINDRICAL_SURFACE ( 'NONE', #3285, 60.74260934110282051 ) ;
#6643 = DIRECTION ( 'NONE',  ( 0.000000000000000000, 0.000000000000000000, 1.000000000000000000 ) ) ;
#6644 = ORIENTED_EDGE ( 'NONE', *, *, #4772, .F. ) ;
#6645 = DIRECTION ( 'NONE',  ( 0.1390141521205912056, -0.9902903945359629034, 0.000000000000000000 ) ) ;
#6646 = ORIENTED_EDGE ( 'NONE', *, *, #11299, .T. ) ;
#6647 = EDGE_CURVE ( 'NONE', #4447, #4182, #16885, .T. ) ;
#6648 = AXIS2_PLACEMENT_3D ( 'NONE', #13668, #1403, #13873 ) ;
#6649 = VERTEX_POINT ( 'NONE', #10792 ) ;
#6650 = EDGE_CURVE ( 'NONE', #16844, #18587, #9038, .T. ) ;
#6651 = PLANE ( 'NONE',  #5840 ) ;
#6652 = VERTEX_POINT ( 'NONE', #6210 ) ;
#6653 = B_SPLINE_CURVE_WITH_KNOTS ( 'NONE', 3,
 ( #12593, #15685, #11165, #1457, #7893, #1761, #2997, #11064, #8094, #9330, #6278, #7686, #12700, #1666, #4524, #9636, #10958, #13928, #18652, #20173, #12393, #18855, #7996, #12491, #17219, #3200 ),
 .UNSPECIFIED., .F., .F.,
 ( 4, 2, 2, 2, 2, 2, 2, 2, 2, 2, 2, 2, 4 ),
 ( 0.000000000000000000, 0.001429785831555309026, 0.002144678747332965599, 0.002859571663110624992, 0.004289357494665932066, 0.005719143326221240442, 0.007148929157776548818, 0.008578714989331853724, 0.01143828665244240976, 0.01429785831555296580, 0.01572764414710824468, 0.01715742997866355479, 0.02287657330488494789 ),
 .UNSPECIFIED. ) ;
#6654 = CARTESIAN_POINT ( 'NONE',  ( 120.7779226595530986, 102.2982297021113141, 60.00000000000000000 ) ) ;
#6655 = DIRECTION ( 'NONE',  ( 1.000000000000000000, 0.000000000000000000, -0.000000000000000000 ) ) ;
#6656 = VECTOR ( 'NONE', #19449, 1000.000000000000227 ) ;
#6657 = ORIENTED_EDGE ( 'NONE', *, *, #3104, .T. ) ;
#6658 = VECTOR ( 'NONE', #11378, 999.9999999999998863 ) ;
#6659 =( LENGTH_UNIT ( ) NAMED_UNIT ( * ) SI_UNIT ( .MILLI., .METRE. ) );
#6660 = CYLINDRICAL_SURFACE ( 'NONE', #17825, 7.500000000000020428 ) ;
#6661 = LINE ( 'NONE', #12295, #11145 ) ;
#6662 = EDGE_CURVE ( 'NONE', #16938, #2113, #13773, .T. ) ;
#6663 = DIRECTION ( 'NONE',  ( -0.000000000000000000, -0.000000000000000000, 1.000000000000000000 ) ) ;
#6664 = AXIS2_PLACEMENT_3D ( 'NONE', #11876, #10549, #2897 ) ;
#6665 = CARTESIAN_POINT ( 'NONE',  ( 37.78198917157320125, -47.56244194535178593, 283.5832628385307999 ) ) ;
#6666 = DIRECTION ( 'NONE',  ( -0.000000000000000000, -0.000000000000000000, 1.000000000000000000 ) ) ;
#6667 = VERTEX_POINT ( 'NONE', #13961 ) ;
#6668 = PLANE ( 'NONE',  #9567 ) ;
#6669 = LINE ( 'NONE', #1748, #1874 ) ;
#6670 = DIRECTION ( 'NONE',  ( -0.03505990758545545621, -0.9993852124581888985, 0.000000000000000000 ) ) ;
#6671 = CARTESIAN_POINT ( 'NONE',  ( 106.9434821670232623, -119.5159909196223111, 40.00000000000000000 ) ) ;
#6672 = EDGE_LOOP ( 'NONE', ( #4056, #14230, #918, #12943 ) ) ;
#6673 = DIRECTION ( 'NONE',  ( -0.1736481776669241417, -0.9848077530122091305, 0.000000000000000000 ) ) ;
#6674 = DIRECTION ( 'NONE',  ( -0.000000000000000000, -0.000000000000000000, 1.000000000000000000 ) ) ;
#6675 = EDGE_CURVE ( 'NONE', #5793, #13282, #7419, .T. ) ;
#6676 = VERTEX_POINT ( 'NONE', #9364 ) ;
#6677 = ADVANCED_FACE ( 'NONE', ( #13656 ), #1596, .F. ) ;
#6678 = ORIENTED_EDGE ( 'NONE', *, *, #10648, .F. ) ;
#6679 = ORIENTED_EDGE ( 'NONE', *, *, #11610, .F. ) ;
#6680 = PRODUCT_CONTEXT ( 'NONE', #17190, 'mechanical' ) ;
#6681 = VECTOR ( 'NONE', #17116, 999.9999999999998863 ) ;
#6682 = ORIENTED_EDGE ( 'NONE', *, *, #12825, .T. ) ;
#6683 = ADVANCED_FACE ( 'NONE', ( #20103 ), #6101, .F. ) ;
#6684 = DIRECTION ( 'NONE',  ( 0.000000000000000000, 0.000000000000000000, 1.000000000000000000 ) ) ;
#6685 = ORIENTED_EDGE ( 'NONE', *, *, #12462, .F. ) ;
#6686 = FILL_AREA_STYLE ('',( #1975 ) ) ;
#6687 = DIRECTION ( 'NONE',  ( -0.9993852124581887875, 0.03505990758545545621, 0.000000000000000000 ) ) ;
#6688 = CARTESIAN_POINT ( 'NONE',  ( -82.57283217324577151, -125.2267376009800444, 5.213532245358446282 ) ) ;
#6689 = FACE_OUTER_BOUND ( 'NONE', #17347, .T. ) ;
#6690 = PLANE ( 'NONE',  #1098 ) ;
#6691 = DIRECTION ( 'NONE',  ( -0.6155349844899689060, 0.7881095627315620744, 0.000000000000000000 ) ) ;
#6692 = CIRCLE ( 'NONE', #20065, 62.91752772691707207 ) ;
#6693 = CARTESIAN_POINT ( 'NONE',  ( 0.000000000000000000, 0.000000000000000000, 293.5832628385307999 ) ) ;
#6694 = CARTESIAN_POINT ( 'NONE',  ( 0.000000000000000000, 0.000000000000000000, -100.0000000000000000 ) ) ;
#6695 = CARTESIAN_POINT ( 'NONE',  ( 0.000000000000000000, 0.000000000000000000, 0.000000000000000000 ) ) ;
#6696 = VERTEX_POINT ( 'NONE', #7825 ) ;
#6697 = CARTESIAN_POINT ( 'NONE',  ( -128.5162560489251860, 45.03435910158038524, -24.76419096631276417 ) ) ;
#6698 = AXIS2_PLACEMENT_3D ( 'NONE', #2222, #17973, #6724 ) ;
#6699 = ORIENTED_EDGE ( 'NONE', *, *, #492, .T. ) ;
#6700 = VERTEX_POINT ( 'NONE', #57 ) ;
#6701 = VERTEX_POINT ( 'NONE', #18270 ) ;
#6702 = VECTOR ( 'NONE', #15845, 1000.000000000000114 ) ;
#6703 = FACE_OUTER_BOUND ( 'NONE', #17301, .T. ) ;
#6704 = LINE ( 'NONE', #8531, #7650 ) ;
#6705 = CARTESIAN_POINT ( 'NONE',  ( -28.63313560863435825, 51.23821591265124198, 132.4711112102474146 ) ) ;
#6706 = DIRECTION ( 'NONE',  ( -0.9009688679024160374, -0.4338837391175646707, 0.000000000000000000 ) ) ;
#6707 = CARTESIAN_POINT ( 'NONE',  ( 0.000000000000000000, 0.000000000000000000, 293.5832628385307999 ) ) ;
#6708 = ORIENTED_EDGE ( 'NONE', *, *, #6244, .T. ) ;
#6709 = DIRECTION ( 'NONE',  ( -1.000000000000000000, 0.000000000000000000, 0.000000000000000000 ) ) ;
#6710 = LINE ( 'NONE', #12527, #12145 ) ;
#6711 = FACE_OUTER_BOUND ( 'NONE', #15002, .T. ) ;
#6712 = CARTESIAN_POINT ( 'NONE',  ( -41.06890862491506766, -47.66508197439458172, 132.4711112102474146 ) ) ;
#6713 = LINE ( 'NONE', #6812, #4836 ) ;
#6714 = ORIENTED_EDGE ( 'NONE', *, *, #15135, .T. ) ;
#6715 = AXIS2_PLACEMENT_3D ( 'NONE', #3619, #15898, #8110 ) ;
#6716 = CARTESIAN_POINT ( 'NONE',  ( 134.1103769904815408, -77.28650662340041322, 36.11580906139592173 ) ) ;
#6717 = VERTEX_POINT ( 'NONE', #10478 ) ;
#6718 = ORIENTED_EDGE ( 'NONE', *, *, #2523, .T. ) ;
#6719 = ORIENTED_EDGE ( 'NONE', *, *, #13494, .F. ) ;
#6720 = VERTEX_POINT ( 'NONE', #17250 ) ;
#6721 = EDGE_CURVE ( 'NONE', #10957, #18684, #17460, .T. ) ;
#6722 = ORIENTED_EDGE ( 'NONE', *, *, #7504, .T. ) ;
#6723 = DIRECTION ( 'NONE',  ( -0.6692498792541753394, -0.7430374143461900838, 0.000000000000000000 ) ) ;
#6724 = DIRECTION ( 'NONE',  ( 1.000000000000000000, 3.491481338843133355E-15, 0.000000000000000000 ) ) ;
#6725 = CARTESIAN_POINT ( 'NONE',  ( 0.000000000000000000, 0.000000000000000000, -120.0000000000000142 ) ) ;
#6726 = VERTEX_POINT ( 'NONE', #6408 ) ;
#6727 = APPLICATION_CONTEXT ( 'automotive_design' ) ;
#6728 = PLANE ( 'NONE',  #5391 ) ;
#6729 = DIRECTION ( 'NONE',  ( 1.000000000000000000, 0.000000000000000000, -6.994638739193269649E-15 ) ) ;
#6730 = ORIENTED_EDGE ( 'NONE', *, *, #12968, .T. ) ;
#6731 = EDGE_CURVE ( 'NONE', #20085, #7290, #11169, .T. ) ;
#6732 = DIRECTION ( 'NONE',  ( -0.000000000000000000, -0.000000000000000000, 1.000000000000000000 ) ) ;
#6733 = FACE_OUTER_BOUND ( 'NONE', #17083, .T. ) ;
#6734 = CARTESIAN_POINT ( 'NONE',  ( -17.24542129382105315, 20.55229278271246329, 39.88498244535557546 ) ) ;
#6735 = AXIS2_PLACEMENT_3D ( 'NONE', #11523, #11710, #16338 ) ;
#6736 = ADVANCED_FACE ( 'NONE', ( #18890 ), #15712, .F. ) ;
#6737 = DIRECTION ( 'NONE',  ( 0.000000000000000000, 0.000000000000000000, 1.000000000000000000 ) ) ;
#6738 = DIRECTION ( 'NONE',  ( -0.000000000000000000, -0.000000000000000000, 1.000000000000000000 ) ) ;
#6739 = DIRECTION ( 'NONE',  ( -0.000000000000000000, -0.000000000000000000, 1.000000000000000000 ) ) ;
#6740 = CARTESIAN_POINT ( 'NONE',  ( 87.33261371895460456, -121.9603527571197361, 43.99921538561949319 ) ) ;
#6741 = ORIENTED_EDGE ( 'NONE', *, *, #10759, .T. ) ;
#6742 = VECTOR ( 'NONE', #4373, 1000.000000000000000 ) ;
#6743 = CYLINDRICAL_SURFACE ( 'NONE', #5023, 79.75827554147308263 ) ;
#6744 = VERTEX_POINT ( 'NONE', #7923 ) ;
#6745 = ORIENTED_EDGE ( 'NONE', *, *, #7717, .T. ) ;
#6746 = EDGE_CURVE ( 'NONE', #6652, #959, #3432, .T. ) ;
#6747 = DIRECTION ( 'NONE',  ( -0.000000000000000000, -1.000000000000000000, -0.000000000000000000 ) ) ;
#6748 = ORIENTED_EDGE ( 'NONE', *, *, #4611, .F. ) ;
#6749 = VECTOR ( 'NONE', #17043, 1000.000000000000000 ) ;
#6750 = CARTESIAN_POINT ( 'NONE',  ( 7.500000000000008882, 164.0736214083062805, 49.99999999999999289 ) ) ;
#6751 = AXIS2_PLACEMENT_3D ( 'NONE', #2998, #17112, #3098 ) ;
#6752 = DIRECTION ( 'NONE',  ( 1.000000000000000000, 0.000000000000000000, 0.000000000000000000 ) ) ;
#6753 = DIRECTION ( 'NONE',  ( -1.000000000000000000, 0.000000000000000000, 0.000000000000000000 ) ) ;
#6754 = DIRECTION ( 'NONE',  ( 0.000000000000000000, 0.000000000000000000, 1.000000000000000000 ) ) ;
#6755 = CARTESIAN_POINT ( 'NONE',  ( -61.70726652483826058, -12.28122767885825262, 248.9926560891072143 ) ) ;
#6756 = EDGE_CURVE ( 'NONE', #13973, #6205, #6609, .T. ) ;
#6757 = CARTESIAN_POINT ( 'NONE',  ( -57.61627707419551570, -19.23614321207253042, 283.5832628385307999 ) ) ;
#6758 = EDGE_CURVE ( 'NONE', #4372, #17725, #4650, .T. ) ;
#6759 = DIRECTION ( 'NONE',  ( -0.9848077530122073542, -0.1736481776669340227, -0.000000000000000000 ) ) ;
#6760 = EDGE_CURVE ( 'NONE', #19007, #11829, #6297, .T. ) ;
#6761 = DIRECTION ( 'NONE',  ( -8.294538580027652572E-17, 2.273402209432136919E-16, -1.000000000000000000 ) ) ;
#6762 = EDGE_LOOP ( 'NONE', ( #5044, #5959, #1101, #3246 ) ) ;
#6763 = CYLINDRICAL_SURFACE ( 'NONE', #7596, 60.74260934110282051 ) ;
#6764 = DIRECTION ( 'NONE',  ( 1.000000000000000000, 0.000000000000000000, 0.000000000000000000 ) ) ;
#6765 = CARTESIAN_POINT ( 'NONE',  ( 89.19226148815698707, -120.6070458769191163, -5.778503507065541278 ) ) ;
#6766 = CARTESIAN_POINT ( 'NONE',  ( 100.7812500000000284, -111.0996833858562809, 39.99999999999999289 ) ) ;
#6767 = AXIS2_PLACEMENT_3D ( 'NONE', #12658, #5204, #18920 ) ;
#6768 = ORIENTED_EDGE ( 'NONE', *, *, #10223, .F. ) ;
#6769 = CIRCLE ( 'NONE', #2506, 3.224098631618459443 ) ;
#6770 = CARTESIAN_POINT ( 'NONE',  ( 15.91767397667354089, 149.1530343478547422, 60.00000000000000000 ) ) ;
#6771 = CARTESIAN_POINT ( 'NONE',  ( -99.66897253883981023, 112.1566004585619964, 43.73620438184401138 ) ) ;
#6772 = VERTEX_POINT ( 'NONE', #6514 ) ;
#6773 = EDGE_LOOP ( 'NONE', ( #19048, #16599, #327, #16030 ) ) ;
#6775 = VERTEX_POINT ( 'NONE', #2104 ) ;
#6774 = AXIS2_PLACEMENT_3D ( 'NONE', #1652, #8080, #14227 ) ;
#6776 = EDGE_CURVE ( 'NONE', #5779, #9877, #158, .T. ) ;
#6777 = ORIENTED_EDGE ( 'NONE', *, *, #5251, .T. ) ;
#6778 = EDGE_CURVE ( 'NONE', #2503, #573, #19091, .T. ) ;
#6779 = DIRECTION ( 'NONE',  ( -1.000000000000000000, 0.000000000000000000, 0.000000000000000000 ) ) ;
#6780 = CARTESIAN_POINT ( 'NONE',  ( -73.82206860051547892, -25.99419088092166774, 111.4180192758973931 ) ) ;
#6781 = VERTEX_POINT ( 'NONE', #12628 ) ;
#6782 = CYLINDRICAL_SURFACE ( 'NONE', #8666, 7.500000000000003553 ) ;
#6783 = DIRECTION ( 'NONE',  ( 0.000000000000000000, 0.000000000000000000, 1.000000000000000000 ) ) ;
#6784 = CARTESIAN_POINT ( 'NONE',  ( -87.54876440220090217, -121.8053786065146511, -4.230840218062975389 ) ) ;
#6785 = ORIENTED_EDGE ( 'NONE', *, *, #17449, .T. ) ;
#6786 = EDGE_CURVE ( 'NONE', #2414, #4265, #1373, .T. ) ;
#6787 = EDGE_CURVE ( 'NONE', #19395, #5114, #14276, .T. ) ;
#6788 = EDGE_CURVE ( 'NONE', #9930, #9275, #12733, .T. ) ;
#6789 = LINE ( 'NONE', #827, #2952 ) ;
#6790 = DIRECTION ( 'NONE',  ( -0.000000000000000000, -0.000000000000000000, 1.000000000000000000 ) ) ;
#6791 = CIRCLE ( 'NONE', #17240, 62.91752772691707207 ) ;
#6792 = DIRECTION ( 'NONE',  ( 6.982962677686266711E-15, -0.000000000000000000, 1.000000000000000000 ) ) ;
#6793 = PLANE ( 'NONE',  #3917 ) ;
#6794 = FACE_OUTER_BOUND ( 'NONE', #12998, .T. ) ;
#6795 = CARTESIAN_POINT ( 'NONE',  ( 81.66698895276897474, 79.37254397626031732, 39.88498244535488624 ) ) ;
#6796 = ORIENTED_EDGE ( 'NONE', *, *, #750, .F. ) ;
#6797 = LINE ( 'NONE', #12817, #8242 ) ;
#6798 = EDGE_LOOP ( 'NONE', ( #969, #9593, #17261, #1817, #16224, #2508 ) ) ;
#6799 = CIRCLE ( 'NONE', #3832, 6.000000000000001776 ) ;
#6800 = ORIENTED_EDGE ( 'NONE', *, *, #61, .F. ) ;
#6801 = CIRCLE ( 'NONE', #9406, 60.74260934110282051 ) ;
#6802 = VERTEX_POINT ( 'NONE', #2004 ) ;
#6803 = LINE ( 'NONE', #8625, #14821 ) ;
#6804 = CARTESIAN_POINT ( 'NONE',  ( -135.0831964404853238, -65.21150773178311510, 8.539806532481302170 ) ) ;
#6805 = DIRECTION ( 'NONE',  ( -1.000000000000000000, 0.000000000000000000, 0.000000000000000000 ) ) ;
#6806 = EDGE_CURVE ( 'NONE', #11084, #10879, #1897, .T. ) ;
#6807 = PLANE ( 'NONE',  #2291 ) ;
#6808 = DIRECTION ( 'NONE',  ( -0.1736481776669241417, -0.9848077530122091305, -0.000000000000000000 ) ) ;
#6809 = CARTESIAN_POINT ( 'NONE',  ( 133.9275976130212200, -67.55320356804583071, 1.164109098278201193 ) ) ;
#6810 = CARTESIAN_POINT ( 'NONE',  ( -60.68567895461851691, 2.629250726500500956, 283.5832628385307999 ) ) ;
#6811 = CARTESIAN_POINT ( 'NONE',  ( 99.09522870387660021, -131.8160711339301372, 35.43273011591471544 ) ) ;
#6812 = CARTESIAN_POINT ( 'NONE',  ( 26.55444175051045974, 16.92388544840595799, 248.9926560891072143 ) ) ;
#6813 = AXIS2_PLACEMENT_3D ( 'NONE', #19087, #5074, #18989 ) ;
#6814 = EDGE_CURVE ( 'NONE', #399, #17740, #8130, .T. ) ;
#6815 = ORIENTED_EDGE ( 'NONE', *, *, #18096, .F. ) ;
#6816 = AXIS2_PLACEMENT_3D ( 'NONE', #3692, #8593, #9931 ) ;
#6817 = ORIENTED_EDGE ( 'NONE', *, *, #15413, .F. ) ;
#6818 = ORIENTED_EDGE ( 'NONE', *, *, #9505, .T. ) ;
#6819 = VERTEX_POINT ( 'NONE', #355 ) ;
#6820 = CIRCLE ( 'NONE', #15335, 15.91767397667355510 ) ;
#6821 = ORIENTED_EDGE ( 'NONE', *, *, #20022, .F. ) ;
#6822 = VECTOR ( 'NONE', #19380, 1000.000000000000227 ) ;
#6823 = CIRCLE ( 'NONE', #16952, 62.91752772691707207 ) ;
#6824 = CARTESIAN_POINT ( 'NONE',  ( 59.42266395395792955, -50.93469132750283279, 248.9926560891072143 ) ) ;
#6825 = AXIS2_PLACEMENT_3D ( 'NONE', #18617, #18309, #4595 ) ;
#6826 = DIRECTION ( 'NONE',  ( -0.8660254037844328234, -0.5000000000000101030, 0.000000000000000000 ) ) ;
#6827 = CARTESIAN_POINT ( 'NONE',  ( 38.35506425062457225, 44.43084819159290788, 132.4711112102474146 ) ) ;
#6828 = VERTEX_POINT ( 'NONE', #12832 ) ;
#6829 = DIRECTION ( 'NONE',  ( 0.9009688679024218105, -0.4338837391175526248, 0.000000000000000000 ) ) ;
#6830 = DIRECTION ( 'NONE',  ( 0.9848077530122086864, -0.1736481776669273613, -0.000000000000000000 ) ) ;
#6831 = ORIENTED_EDGE ( 'NONE', *, *, #19362, .F. ) ;
#6832 = CARTESIAN_POINT ( 'NONE',  ( -95.84941630392641798, 106.2995539097782824, -32.42387014996108263 ) ) ;
#6833 = DIRECTION ( 'NONE',  ( 0.9396926207859104263, 0.3420201433256630508, -6.561838499445206374E-15 ) ) ;
#6834 = CARTESIAN_POINT ( 'NONE',  ( 134.7188131032333445, -72.93593548660993520, 10.00000000000000178 ) ) ;
#6835 = DIRECTION ( 'NONE',  ( 0.000000000000000000, 0.000000000000000000, -1.000000000000000000 ) ) ;
#6836 = DIRECTION ( 'NONE',  ( -6.982962677686266711E-15, 0.000000000000000000, -1.000000000000000000 ) ) ;
#6837 = CARTESIAN_POINT ( 'NONE',  ( 84.97262318626000877, -123.6115503146182277, 40.77684021904739353 ) ) ;
#6838 = AXIS2_PLACEMENT_3D ( 'NONE', #20234, #19022, #7952 ) ;
#6839 = VECTOR ( 'NONE', #6830, 999.9999999999998863 ) ;
#6840 = EDGE_LOOP ( 'NONE', ( #18224, #3984, #1245, #17665 ) ) ;
#6841 = DIRECTION ( 'NONE',  ( 0.000000000000000000, 1.000000000000000000, 0.000000000000000000 ) ) ;
#6842 = ORIENTED_EDGE ( 'NONE', *, *, #7746, .T. ) ;
#6843 = ORIENTED_EDGE ( 'NONE', *, *, #15595, .T. ) ;
#6844 = CARTESIAN_POINT ( 'NONE',  ( 54.89456854707540856, 30.74413178637211885, 132.4711112102474146 ) ) ;
#6845 = ORIENTED_EDGE ( 'NONE', *, *, #10383, .T. ) ;
#6846 = CARTESIAN_POINT ( 'NONE',  ( 20.21777810286676313, 59.58067424803633116, 132.4711112102474146 ) ) ;
#6847 = CARTESIAN_POINT ( 'NONE',  ( -84.32000978867637286, -124.0571233621915610, 39.58209758642278331 ) ) ;
#6848 = SURFACE_SIDE_STYLE ('',( #15861 ) ) ;
#6849 = DIRECTION ( 'NONE',  ( 1.000000000000000000, 0.000000000000000000, 0.000000000000000000 ) ) ;
#6850 = VECTOR ( 'NONE', #17659, 1000.000000000000000 ) ;
#6851 = VERTEX_POINT ( 'NONE', #8227 ) ;
#6852 = CARTESIAN_POINT ( 'NONE',  ( 0.000000000000000000, 0.000000000000000000, -40.00000000000000000 ) ) ;
#6853 = CARTESIAN_POINT ( 'NONE',  ( 107.5000000000000142, -118.5063289449133492, 0.000000000000000000 ) ) ;
#6854 = EDGE_CURVE ( 'NONE', #18461, #18497, #14474, .T. ) ;
#6855 = CARTESIAN_POINT ( 'NONE',  ( 141.8714406926368099, -48.70825716237079916, 49.99999999999999289 ) ) ;
#6856 = DIRECTION ( 'NONE',  ( 0.9396926207859058744, -0.3420201433256757073, -6.562243095054852012E-15 ) ) ;
#6857 = EDGE_CURVE ( 'NONE', #6064, #7509, #6710, .T. ) ;
#6858 = VERTEX_POINT ( 'NONE', #3635 ) ;
#6859 = DIRECTION ( 'NONE',  ( 1.047444401652940164E-14, -1.000000000000000000, 0.000000000000000000 ) ) ;
#6860 = DIRECTION ( 'NONE',  ( -1.000000000000000000, 0.000000000000000000, 0.000000000000000000 ) ) ;
#6861 = CARTESIAN_POINT ( 'NONE',  ( -62.09913334491130144, -10.11498556985140596, 248.9926560891072143 ) ) ;
#6862 = DIRECTION ( 'NONE',  ( -0.1736481776669273336, -0.9848077530122085754, 0.000000000000000000 ) ) ;
#6863 = ORIENTED_EDGE ( 'NONE', *, *, #11265, .F. ) ;
#6864 = PLANE ( 'NONE',  #12684 ) ;
#6865 = LINE ( 'NONE', #16286, #19063 ) ;
#6866 = ORIENTED_EDGE ( 'NONE', *, *, #7749, .F. ) ;
#6867 = ORIENTED_EDGE ( 'NONE', *, *, #17624, .T. ) ;
#6868 = ORIENTED_EDGE ( 'NONE', *, *, #13101, .F. ) ;
#6869 = ITEM_DEFINED_TRANSFORMATION ( 'NONE', 'NONE', #9850,  #18639 ) ;
#6870 = ADVANCED_FACE ( 'NONE', ( #9865 ), #18787, .T. ) ;
#6871 = EDGE_CURVE ( 'NONE', #13282, #241, #2498, .T. ) ;
#6873 = ORIENTED_EDGE ( 'NONE', *, *, #8272, .T. ) ;
#6872 = VECTOR ( 'NONE', #16076, 1000.000000000000000 ) ;
#6874 = EDGE_CURVE ( 'NONE', #4648, #9930, #19388, .T. ) ;
#6875 = DIRECTION ( 'NONE',  ( 0.000000000000000000, 0.000000000000000000, 1.000000000000000000 ) ) ;
#6876 = DIRECTION ( 'NONE',  ( 0.000000000000000000, 0.000000000000000000, 1.000000000000000000 ) ) ;
#6877 = ORIENTED_EDGE ( 'NONE', *, *, #740, .F. ) ;
#6878 = DIRECTION ( 'NONE',  ( 0.000000000000000000, 0.000000000000000000, -1.000000000000000000 ) ) ;
#6879 = LINE ( 'NONE', #636, #15154 ) ;
#6880 = CARTESIAN_POINT ( 'NONE',  ( -97.11506731898813882, -115.6376992562254742, 10.35708075459104371 ) ) ;
#6881 = AXIS2_PLACEMENT_3D ( 'NONE', #13378, #5621, #617 ) ;
#6882 = ORIENTED_EDGE ( 'NONE', *, *, #9505, .F. ) ;
#6883 = CIRCLE ( 'NONE', #13711, 62.91752772691707207 ) ;
#6884 = EDGE_CURVE ( 'NONE', #4813, #19147, #8538, .T. ) ;
#6885 = CARTESIAN_POINT ( 'NONE',  ( -5.951998377315654842, -25.21111933077039069, 14.88498244535549198 ) ) ;
#6886 = CYLINDRICAL_SURFACE ( 'NONE', #15431, 3.224098631618460331 ) ;
#6887 = DIRECTION ( 'NONE',  ( 0.4999999999999888978, 0.8660254037844449249, 0.000000000000000000 ) ) ;
#6888 = CARTESIAN_POINT ( 'NONE',  ( -39.80940113485987553, 48.72193424476490975, 248.9926560891072143 ) ) ;
#6889 = CARTESIAN_POINT ( 'NONE',  ( -54.89456854707562172, -30.74413178637172450, 293.5832628385307999 ) ) ;
#6890 = EDGE_LOOP ( 'NONE', ( #5185, #17513, #19459, #12904 ) ) ;
#6891 = DIRECTION ( 'NONE',  ( -1.000000000000000000, 0.000000000000000000, 0.000000000000000000 ) ) ;
#6892 = CIRCLE ( 'NONE', #3305, 62.91752772691707207 ) ;
#6893 = ORIENTED_EDGE ( 'NONE', *, *, #19551, .T. ) ;
#6894 = ADVANCED_FACE ( 'NONE', ( #13320 ), #13422, .F. ) ;
#6895 = EDGE_CURVE ( 'NONE', #16743, #11013, #10356, .T. ) ;
#6896 = ORIENTED_EDGE ( 'NONE', *, *, #18633, .F. ) ;
#6897 = EDGE_CURVE ( 'NONE', #6948, #6452, #5619, .T. ) ;
#6898 = PRODUCT_RELATED_PRODUCT_CATEGORY ( 'part', '', ( #9652 ) ) ;
#6900 = VERTEX_POINT ( 'NONE', #757 ) ;
#6899 = B_SPLINE_CURVE_WITH_KNOTS ( 'NONE', 3,
 ( #5935, #9084, #4384, #12148, #12354, #2961, #15645, #20037, #10820, #15327, #12456, #6136, #9191, #15221, #18718, #4701, #15434, #16765, #1206, #12560, #1425, #20135, #18409, #4284, #18613, #1525, #17076, #3066, #9299, #3167, #10509, #15543, #13996, #10926, #17592, #16052, #5110, #4913, #3365, #5012, #9903, #1722, #15743, #3667, #18926, #7960, #11339, #8363 ),
 .UNSPECIFIED., .F., .F.,
 ( 4, 2, 2, 2, 2, 2, 2, 2, 2, 2, 2, 2, 2, 2, 2, 2, 2, 2, 2, 2, 2, 2, 2, 4 ),
 ( 0.09493486412272097996, 0.09745231401683318584, 0.09996976391094537784, 0.1050046636991697896, 0.1150744632756185853, 0.1201093630638430110, 0.1226268129579552169, 0.1251442628520674227, 0.1301791626402918900, 0.1326966125344041236, 0.1352140624285163295, 0.1402489622167407690, 0.1452838620049651808, 0.1478013118990773589, 0.1503187617931895925, 0.1553536615814139765, 0.1566123865284700933, 0.1578711114755261824, 0.1603885613696383605, 0.1654234611578627445, 0.1666821861049188613, 0.1679409110519749504, 0.1704583609460871285, 0.1754932607343114848 ),
 .UNSPECIFIED. ) ;
#6901 = DIRECTION ( 'NONE',  ( 0.000000000000000000, 0.000000000000000000, 1.000000000000000000 ) ) ;
#6902 = CARTESIAN_POINT ( 'NONE',  ( -124.4460166144179141, -83.75677717049846649, -9.878997880596227077 ) ) ;
#6903 = CARTESIAN_POINT ( 'NONE',  ( -189.9999999999988916, 275.0000000000000000, 5.000000000000268230 ) ) ;
#6904 = FACE_OUTER_BOUND ( 'NONE', #10463, .T. ) ;
#6905 = VERTEX_POINT ( 'NONE', #2603 ) ;
#6906 = DIRECTION ( 'NONE',  ( 1.000000000000000000, 0.000000000000000000, 0.000000000000000000 ) ) ;
#6907 = CARTESIAN_POINT ( 'NONE',  ( -131.5441688916725980, -89.82688951535520516, 0.05736369426573884045 ) ) ;
#6908 = AXIS2_PLACEMENT_3D ( 'NONE', #8411, #544, #16493 ) ;
#6909 = EDGE_CURVE ( 'NONE', #5912, #380, #9970, .T. ) ;
#6910 = CARTESIAN_POINT ( 'NONE',  ( 134.7221128596253550, -65.95429948960817512, 4.840168302597956718 ) ) ;
#6911 = CYLINDRICAL_SURFACE ( 'NONE', #8795, 7.500000000000000000 ) ;
#6912 = DIRECTION ( 'NONE',  ( 1.000000000000000000, 0.000000000000000000, 0.000000000000000000 ) ) ;
#6913 = AXIS2_PLACEMENT_3D ( 'NONE', #11600, #3829, #4029 ) ;
#6914 = FACE_OUTER_BOUND ( 'NONE', #4816, .T. ) ;
#6915 = ORIENTED_EDGE ( 'NONE', *, *, #6650, .F. ) ;
#6916 = ORIENTED_EDGE ( 'NONE', *, *, #15464, .T. ) ;
#6917 = VERTEX_POINT ( 'NONE', #8435 ) ;
#6918 = EDGE_CURVE ( 'NONE', #2266, #12685, #17959, .T. ) ;
#6919 = EDGE_CURVE ( 'NONE', #6819, #1, #16220, .T. ) ;
#6920 = ORIENTED_EDGE ( 'NONE', *, *, #19168, .T. ) ;
#6921 = ORIENTED_EDGE ( 'NONE', *, *, #9023, .T. ) ;
#6922 = ADVANCED_FACE ( 'NONE', ( #8729 ), #8338, .F. ) ;
#6923 = CARTESIAN_POINT ( 'NONE',  ( 56.12853591711344592, -23.22718332831461652, 293.5832628385307999 ) ) ;
#6924 = CARTESIAN_POINT ( 'NONE',  ( 138.2024300533213932, 89.85329105948596862, 39.99999999999999289 ) ) ;
#6925 = CARTESIAN_POINT ( 'NONE',  ( 0.000000000000000000, 0.000000000000000000, 283.5832628385307999 ) ) ;
#6926 = VERTEX_POINT ( 'NONE', #4230 ) ;
#6927 = CARTESIAN_POINT ( 'NONE',  ( 51.24245927909996112, -32.62092819947974220, 293.5832628385307999 ) ) ;
#6928 = CARTESIAN_POINT ( 'NONE',  ( -62.09913334491130854, -10.11498556985139352, 132.4711112102474146 ) ) ;
#6929 = ORIENTED_EDGE ( 'NONE', *, *, #4244, .F. ) ;
#6930 = CARTESIAN_POINT ( 'NONE',  ( -97.59206265536077751, 66.04728469612305730, 14.88498244535613146 ) ) ;
#6931 = DIRECTION ( 'NONE',  ( 6.982962677686266711E-15, -0.000000000000000000, 1.000000000000000000 ) ) ;
#6932 = FACE_OUTER_BOUND ( 'NONE', #14977, .T. ) ;
#6933 = CARTESIAN_POINT ( 'NONE',  ( 74.01264520835154315, -25.47058595421579241, 248.9926560891072143 ) ) ;
#6934 = DIRECTION ( 'NONE',  ( -6.982962677686266711E-15, 0.000000000000000000, -1.000000000000000000 ) ) ;
#6935 = LINE ( 'NONE', #13154, #6304 ) ;
#6936 = CARTESIAN_POINT ( 'NONE',  ( 113.3640620605769413, -25.59923667990641150, 14.88498244535466064 ) ) ;
#6937 = EDGE_LOOP ( 'NONE', ( #12236, #19592, #7688 ) ) ;
#6938 = DIRECTION ( 'NONE',  ( 0.000000000000000000, 0.000000000000000000, 1.000000000000000000 ) ) ;
#6939 = VECTOR ( 'NONE', #1694, 1000.000000000000000 ) ;
#6940 = ORIENTED_EDGE ( 'NONE', *, *, #16160, .F. ) ;
#6941 = ORIENTED_EDGE ( 'NONE', *, *, #12870, .F. ) ;
#6942 = LINE ( 'NONE', #3764, #9908 ) ;
#6943 = ORIENTED_EDGE ( 'NONE', *, *, #17547, .F. ) ;
#6944 = CARTESIAN_POINT ( 'NONE',  ( 7.500000000000420997, -60.00000000000000000, -105.0000000000000142 ) ) ;
#6945 = CARTESIAN_POINT ( 'NONE',  ( -90.16928584620096387, -119.8796671366212365, 46.53660721316358462 ) ) ;
#6946 = DIRECTION ( 'NONE',  ( 0.9848077530122103518, -0.1736481776669172583, 0.000000000000000000 ) ) ;
#6947 = CYLINDRICAL_SURFACE ( 'NONE', #15187, 62.91752772691707207 ) ;
#6948 = VERTEX_POINT ( 'NONE', #10453 ) ;
#6949 = DIRECTION ( 'NONE',  ( -0.000000000000000000, -0.000000000000000000, 1.000000000000000000 ) ) ;
#6951 = VECTOR ( 'NONE', #9140, 1000.000000000000000 ) ;
#6950 = CARTESIAN_POINT ( 'NONE',  ( 102.1674435767773730, -127.3754966267598405, 1.518799369789654463 ) ) ;
#6952 = CARTESIAN_POINT ( 'NONE',  ( -73.82206860051547892, -25.99419088092166774, 111.4180192758973931 ) ) ;
#6953 = CARTESIAN_POINT ( 'NONE',  ( 79.75827554147308263, 0.000000000000000000, 269.6944534026102360 ) ) ;
#6954 = EDGE_LOOP ( 'NONE', ( #14416, #9655, #5830, #15409 ) ) ;
#6955 = DIRECTION ( 'NONE',  ( -0.000000000000000000, -0.000000000000000000, -1.000000000000000000 ) ) ;
#6956 = LINE ( 'NONE', #11558, #17882 ) ;
#6957 = VECTOR ( 'NONE', #15246, 1000.000000000000000 ) ;
#6958 = FACE_OUTER_BOUND ( 'NONE', #10044, .T. ) ;
#6959 = CYLINDRICAL_SURFACE ( 'NONE', #5639, 15.91767397667354089 ) ;
#6960 = VERTEX_POINT ( 'NONE', #17541 ) ;
#6961 = CARTESIAN_POINT ( 'NONE',  ( 97.51552550667287278, 26.88665364817694581, 14.88498244535477255 ) ) ;
#6962 = LINE ( 'NONE', #5433, #444 ) ;
#6963 = ORIENTED_EDGE ( 'NONE', *, *, #10525, .F. ) ;
#6964 = EDGE_LOOP ( 'NONE', ( #15380, #15492, #4549, #1143 ) ) ;
#6965 = CONTEXT_DEPENDENT_SHAPE_REPRESENTATION ( #17963, #9483 ) ;
#6966 = AXIS2_PLACEMENT_3D ( 'NONE', #19731, #8689, #3892 ) ;
#6967 = AXIS2_PLACEMENT_3D ( 'NONE', #10180, #11426, #677 ) ;
#6968 = EDGE_CURVE ( 'NONE', #11476, #675, #9449, .T. ) ;
#6969 = CARTESIAN_POINT ( 'NONE',  ( 2.240720816136066773, -5.281164089014814600, 293.5832628385307999 ) ) ;
#6970 = EDGE_LOOP ( 'NONE', ( #7535, #9582, #19376, #17099 ) ) ;
#6971 = CIRCLE ( 'NONE', #2717, 7.500000000000020428 ) ;
#6972 = DIRECTION ( 'NONE',  ( -0.000000000000000000, 3.338476886082577323E-16, 1.000000000000000000 ) ) ;
#6973 = CARTESIAN_POINT ( 'NONE',  ( 56.84754764479240663, -154.7316448359447634, 49.99999999999999289 ) ) ;
#6974 = CARTESIAN_POINT ( 'NONE',  ( -95.93567628221582311, -116.0760901523938315, 9.548040410739892181 ) ) ;
#6975 = VERTEX_POINT ( 'NONE', #8008 ) ;
#6976 = CARTESIAN_POINT ( 'NONE',  ( 60.22232964560483737, 7.948937137877944537, 293.5832628385307999 ) ) ;
#6977 = CARTESIAN_POINT ( 'NONE',  ( 0.000000000000000000, 0.000000000000000000, 60.00000000000000000 ) ) ;
#6978 = LINE ( 'NONE', #16587, #11867 ) ;
#6979 = EDGE_CURVE ( 'NONE', #3938, #16337, #3015, .T. ) ;
#6980 = CARTESIAN_POINT ( 'NONE',  ( -62.91752772691707207, 7.705174894103383492E-15, 83.57543755549745867 ) ) ;
#6981 = AXIS2_PLACEMENT_3D ( 'NONE', #11564, #5625, #2168 ) ;
#6982 = EDGE_CURVE ( 'NONE', #14304, #8041, #6290, .T. ) ;
#6983 = CARTESIAN_POINT ( 'NONE',  ( -10.99904278960814352, 0.5388563210140320248, 248.9926560891072143 ) ) ;
#6984 = CYLINDRICAL_SURFACE ( 'NONE', #2917, 27.50000000000000355 ) ;
#6985 = DIRECTION ( 'NONE',  ( 6.982962677686266711E-15, -0.000000000000000000, 1.000000000000000000 ) ) ;
#6986 = ORIENTED_EDGE ( 'NONE', *, *, #13640, .T. ) ;
#6987 = ADVANCED_FACE ( 'NONE', ( #11176 ), #15695, .F. ) ;
#6988 = FACE_OUTER_BOUND ( 'NONE', #7208, .T. ) ;
#6989 = DIRECTION ( 'NONE',  ( -0.2225209339563047894, -0.9749279121818258398, 0.000000000000000000 ) ) ;
#6990 = VECTOR ( 'NONE', #5174, 1000.000000000000000 ) ;
#6991 = CIRCLE ( 'NONE', #16785, 7.500000000000007105 ) ;
#6992 = EDGE_LOOP ( 'NONE', ( #8096, #5554, #16507, #17840 ) ) ;
#6993 = EDGE_CURVE ( 'NONE', #2271, #3721, #10833, .T. ) ;
#6994 = ORIENTED_EDGE ( 'NONE', *, *, #12545, .F. ) ;
#6995 = LINE ( 'NONE', #3629, #12198 ) ;
#6996 = CARTESIAN_POINT ( 'NONE',  ( -122.8001410695374602, -86.14014948502067170, -10.00000000000000178 ) ) ;
#6997 = CARTESIAN_POINT ( 'NONE',  ( 0.000000000000000000, 0.000000000000000000, -10.00000000000000178 ) ) ;
#6998 = AXIS2_PLACEMENT_3D ( 'NONE', #14141, #6072, #10963 ) ;
#6999 = CARTESIAN_POINT ( 'NONE',  ( -27.53920554013687649, -73.25972925305620720, 248.9926560891072143 ) ) ;
#7000 = CARTESIAN_POINT ( 'NONE',  ( 0.000000000000000000, 0.000000000000000000, 293.5832628385307999 ) ) ;
#7001 = VERTEX_POINT ( 'NONE', #10972 ) ;
#7002 = CYLINDRICAL_SURFACE ( 'NONE', #1612, 6.000000000000001776 ) ;
#7003 = CARTESIAN_POINT ( 'NONE',  ( -122.8001410695374744, -86.14014948502068592, -1.214306433183764966E-14 ) ) ;
#7004 = EDGE_CURVE ( 'NONE', #16938, #19717, #9550, .T. ) ;
#7005 = CARTESIAN_POINT ( 'NONE',  ( 134.6956030146747025, -73.12307453597284734, 8.498119811773092280 ) ) ;
#7006 = AXIS2_PLACEMENT_3D ( 'NONE', #12310, #10369, #16827 ) ;
#7007 = EDGE_CURVE ( 'NONE', #16598, #16923, #19661, .T. ) ;
#7008 = CARTESIAN_POINT ( 'NONE',  ( 0.000000000000000000, 0.000000000000000000, 283.5832628385307999 ) ) ;
#7009 = DIRECTION ( 'NONE',  ( -0.3088643371590125697, 0.9511061040868803440, 0.000000000000000000 ) ) ;
#7010 = PRODUCT_DEFINITION_CONTEXT ( 'detailed design', #2931, 'design' ) ;
#7011 = EDGE_CURVE ( 'NONE', #13585, #12690, #2041, .T. ) ;
#7012 = EDGE_LOOP ( 'NONE', ( #425, #819, #1448, #9370 ) ) ;
#7013 = EDGE_LOOP ( 'NONE', ( #11778, #20068, #4726, #14705 ) ) ;
#7014 = EDGE_LOOP ( 'NONE', ( #6554, #20195, #15100, #10720 ) ) ;
#7015 = CIRCLE ( 'NONE', #17486, 9.999999999999994671 ) ;
#7016 = ORIENTED_EDGE ( 'NONE', *, *, #12245, .T. ) ;
#7017 = DIRECTION ( 'NONE',  ( -0.1736481776669172861, -0.9848077530122104628, 0.000000000000000000 ) ) ;
#7018 = EDGE_CURVE ( 'NONE', #19110, #16400, #18975, .T. ) ;
#7019 = EDGE_LOOP ( 'NONE', ( #4887, #4705, #8064, #5986, #1839, #6534 ) ) ;
#7020 = CARTESIAN_POINT ( 'NONE',  ( 0.000000000000000000, 164.0736214083062805, 49.99999999999999289 ) ) ;
#7021 = FACE_BOUND ( 'NONE', #2659, .T. ) ;
#7022 = FACE_OUTER_BOUND ( 'NONE', #15807, .T. ) ;
#7023 = ORIENTED_EDGE ( 'NONE', *, *, #16603, .T. ) ;
#7025 = CARTESIAN_POINT ( 'NONE',  ( -5.485913980968086356, 1.678175111358128024, 293.5832628385307999 ) ) ;
#7024 = VECTOR ( 'NONE', #18632, 1000.000000000000000 ) ;
#7026 = DIRECTION ( 'NONE',  ( -0.000000000000000000, -0.000000000000000000, 1.000000000000000000 ) ) ;
#7027 = ORIENTED_EDGE ( 'NONE', *, *, #11875, .F. ) ;
#7028 = CARTESIAN_POINT ( 'NONE',  ( -37.09555676056967144, 45.48770046196298011, 110.7293897666001214 ) ) ;
#7029 = CARTESIAN_POINT ( 'NONE',  ( 41.02350267428969488, 44.79940644582669051, 293.5832628385307999 ) ) ;
#7030 = DIRECTION ( 'NONE',  ( -0.000000000000000000, -0.000000000000000000, 1.000000000000000000 ) ) ;
#7031 = EDGE_CURVE ( 'NONE', #9870, #11160, #2818, .T. ) ;
#7032 = CIRCLE ( 'NONE', #10272, 9.000000000000000000 ) ;
#7033 = EDGE_CURVE ( 'NONE', #5703, #8191, #19074, .T. ) ;
#7034 = CARTESIAN_POINT ( 'NONE',  ( -45.48770046196285932, -37.09555676056982065, 132.4711112102474146 ) ) ;
#7035 = EDGE_CURVE ( 'NONE', #7429, #10010, #18766, .T. ) ;
#7036 = DIRECTION ( 'NONE',  ( 0.000000000000000000, 0.000000000000000000, 1.000000000000000000 ) ) ;
#7037 = DIRECTION ( 'NONE',  ( -0.3420201433256663259, -0.9396926207859093161, 0.000000000000000000 ) ) ;
#7038 = VERTEX_POINT ( 'NONE', #1676 ) ;
#7039 = EDGE_CURVE ( 'NONE', #12098, #5832, #7251, .T. ) ;
#7040 = CARTESIAN_POINT ( 'NONE',  ( 0.3552109633508538367, -3.484997970623676444, -8.999999999999998224 ) ) ;
#7041 = ADVANCED_FACE ( 'NONE', ( #15589 ), #3315, .F. ) ;
#7042 = ORIENTED_EDGE ( 'NONE', *, *, #11663, .F. ) ;
#7043 = AXIS2_PLACEMENT_3D ( 'NONE', #19435, #9814, #10116 ) ;
#7044 = ORIENTED_EDGE ( 'NONE', *, *, #10414, .F. ) ;
#7045 = CARTESIAN_POINT ( 'NONE',  ( -22.30005961346265408, -56.50329132715937419, 293.5832628385307999 ) ) ;
#7046 = ORIENTED_EDGE ( 'NONE', *, *, #12086, .T. ) ;
#7047 = CARTESIAN_POINT ( 'NONE',  ( 48.09719419928496364, 107.5784105627835174, 14.88498244535511539 ) ) ;
#7048 = CARTESIAN_POINT ( 'NONE',  ( 54.07248341783252954, -32.16802499836759210, 248.9926560891072143 ) ) ;
#7049 = FACE_BOUND ( 'NONE', #20046, .T. ) ;
#7050 = LINE ( 'NONE', #11643, #12905 ) ;
#7051 = CIRCLE ( 'NONE', #18478, 7.500000000000007994 ) ;
#7052 = ORIENTED_EDGE ( 'NONE', *, *, #9797, .T. ) ;
#7053 = CARTESIAN_POINT ( 'NONE',  ( -44.79787735033389851, 41.02212542604627998, 283.5832628385307999 ) ) ;
#7054 = CARTESIAN_POINT ( 'NONE',  ( 98.70372244599823830, -132.3513910121201604, 5.227003128891625217 ) ) ;
#7055 = VECTOR ( 'NONE', #6946, 1000.000000000000000 ) ;
#7056 = CARTESIAN_POINT ( 'NONE',  ( -9.401191644522826962, 61.25984398917663754, 248.9926560891072143 ) ) ;
#7057 = CARTESIAN_POINT ( 'NONE',  ( 3.911853314815645799, -4.196299268919061021, 293.5832628385307999 ) ) ;
#7058 = ORIENTED_EDGE ( 'NONE', *, *, #14021, .T. ) ;
#7059 = FACE_OUTER_BOUND ( 'NONE', #3196, .T. ) ;
#7060 = CARTESIAN_POINT ( 'NONE',  ( -63.68887634719364144, -147.8252249328922687, 60.00000000000000000 ) ) ;
#7061 = CARTESIAN_POINT ( 'NONE',  ( 87.79934266039369106, -121.6207432329495504, -4.446207472610150369 ) ) ;
#7062 = FACE_OUTER_BOUND ( 'NONE', #12799, .T. ) ;
#7063 = EDGE_CURVE ( 'NONE', #4062, #11036, #1573, .T. ) ;
#7064 = ORIENTED_EDGE ( 'NONE', *, *, #12748, .T. ) ;
#7065 = DIRECTION ( 'NONE',  ( 0.9749279121818257288, -0.2225209339563047062, 0.000000000000000000 ) ) ;
#7066 = DIRECTION ( 'NONE',  ( -0.000000000000000000, -0.000000000000000000, 1.000000000000000000 ) ) ;
#7067 = ORIENTED_EDGE ( 'NONE', *, *, #7734, .T. ) ;
#7068 = CIRCLE ( 'NONE', #18496, 32.50000000000000000 ) ;
#7069 = ORIENTED_EDGE ( 'NONE', *, *, #2486, .F. ) ;
#7070 = ORIENTED_EDGE ( 'NONE', *, *, #7772, .F. ) ;
#7071 = LINE ( 'NONE', #5049, #10422 ) ;
#7072 = AXIS2_PLACEMENT_3D ( 'NONE', #7625, #20211, #12433 ) ;
#7073 = DIRECTION ( 'NONE',  ( 0.000000000000000000, 0.000000000000000000, 1.000000000000000000 ) ) ;
#7074 = ORIENTED_EDGE ( 'NONE', *, *, #19168, .F. ) ;
#7075 = CARTESIAN_POINT ( 'NONE',  ( 96.21889527877688408, -115.1753595937449433, 4.451389559091587955 ) ) ;
#7076 = CARTESIAN_POINT ( 'NONE',  ( -103.5930306438084472, -125.1526588151300956, 0.7897485457623537597 ) ) ;
#7077 = VECTOR ( 'NONE', #183, 1000.000000000000000 ) ;
#7078 = CARTESIAN_POINT ( 'NONE',  ( -82.53664710575304753, -125.2505858294166927, 5.373891644490333519 ) ) ;
#7079 = FACE_OUTER_BOUND ( 'NONE', #3599, .T. ) ;
#7080 = CLOSED_SHELL ( 'NONE', ( #19911, #18276, #7955, #15126, #5905, #10987, #5413, #8958, #6396, #10381, #18616, #8105, #14374, #12330, #14108, #4137, #2643, #17443, #3179, #9246, #9891, #18946, #11121, #13316, #10336, #12752, #18272, #8324, #3767, #8241, #13274, #11108, #19742, #4801, #5588, #2898, #16755, #3303, #14780, #15621, #8258, #4104, #15636, #1339, #6268, #17265, #19729, #15476, #7612, #4236, #8159, #19163, #1220, #5499, #13495, #1914, #2760, #2919, #18797, #415, #17924, #8112, #11137, #15991, #19004, #11878, #18733, #16665, #7576, #11281, #12592, #16100, #4655, #7229, #13344, #20140, #11749, #10262, #6987, #5531, #620, #3714, #2139, #871, #16161, #20128, #18288, #7172, #3740, #18660, #654, #13110, #5729, #4107, #13411, #17861, #14515, #4015, #18286, #1038, #12229, #13009, #6922, #1991, #15749, #8163, #16361, #17255, #10228, #3552, #17537, #15844, #19245, #6302, #4390, #13733, #8726, #11481, #12452, #5422, #18655, #15158, #10614, #7616, #13206, #15536, #15516 ) ) ;
#7081 = DIRECTION ( 'NONE',  ( 0.9396926207859046531, 0.3420201433256790380, 0.000000000000000000 ) ) ;
#7082 = CARTESIAN_POINT ( 'NONE',  ( -82.03124999999998579, -125.5821405433014064, 49.99999999999999289 ) ) ;
#7083 = CYLINDRICAL_SURFACE ( 'NONE', #3996, 15.91767397667354800 ) ;
#7084 = DIRECTION ( 'NONE',  ( -0.6155349844899689060, 0.7881095627315620744, 0.000000000000000000 ) ) ;
#7085 = EDGE_CURVE ( 'NONE', #18284, #6828, #2685, .T. ) ;
#7086 = ORIENTED_EDGE ( 'NONE', *, *, #19059, .F. ) ;
#7087 = AXIS2_PLACEMENT_3D ( 'NONE', #6464, #17412, #5135 ) ;
#7088 = LINE ( 'NONE', #18035, #11684 ) ;
#7089 = CARTESIAN_POINT ( 'NONE',  ( -123.8492616149702741, -72.31991210363503342, 10.00000000000000178 ) ) ;
#7090 = EDGE_LOOP ( 'NONE', ( #9408, #6333, #13237 ) ) ;
#7091 = SHAPE_REPRESENTATION_RELATIONSHIP ( 'NONE' , 'NONE' ,  #7558, #1643 ) ;
#7092 = VERTEX_POINT ( 'NONE', #14845 ) ;
#7093 = EDGE_CURVE ( 'NONE', #16460, #371, #5308, .T. ) ;
#7094 = CARTESIAN_POINT ( 'NONE',  ( 22.29928840491074382, 56.50138340076680521, 293.5832628385307999 ) ) ;
#7095 = ORIENTED_EDGE ( 'NONE', *, *, #8274, .T. ) ;
#7096 = CYLINDRICAL_SURFACE ( 'NONE', #451, 3.224098631618460331 ) ;
#7097 = CIRCLE ( 'NONE', #18535, 140.0000000000000000 ) ;
#7098 = DIRECTION ( 'NONE',  ( 1.000000000000000000, 0.000000000000000000, 0.000000000000000000 ) ) ;
#7099 = LINE ( 'NONE', #18045, #19878 ) ;
#7100 = CARTESIAN_POINT ( 'NONE',  ( 77.21438937758502163, 12.78021302872874010, 112.0427633081291816 ) ) ;
#7101 = DIRECTION ( 'NONE',  ( -0.7660444431189707970, -0.6427876096865481337, 0.000000000000000000 ) ) ;
#7102 = DIRECTION ( 'NONE',  ( -1.000000000000000000, 0.000000000000000000, 6.456589605409171438E-15 ) ) ;
#7103 = CARTESIAN_POINT ( 'NONE',  ( 59.30917539369505675, -13.12769224524051559, 283.5832628385307999 ) ) ;
#7104 = FACE_OUTER_BOUND ( 'NONE', #19344, .T. ) ;
#7105 = DIRECTION ( 'NONE',  ( 1.000000000000000000, 0.000000000000000000, 0.000000000000000000 ) ) ;
#7106 = DIRECTION ( 'NONE',  ( 6.982962677686266711E-15, 0.000000000000000000, 1.000000000000000000 ) ) ;
#7107 = EDGE_CURVE ( 'NONE', #6494, #12362, #10506, .T. ) ;
#7108 = VERTEX_POINT ( 'NONE', #16495 ) ;
#7109 =( REPRESENTATION_RELATIONSHIP ('NONE','NONE', #17382, #13949 ) REPRESENTATION_RELATIONSHIP_WITH_TRANSFORMATION ( #5148 )SHAPE_REPRESENTATION_RELATIONSHIP( ) );
#7110 = AXIS2_PLACEMENT_3D ( 'NONE', #7336, #13778, #9072 ) ;
#7112 = ORIENTED_EDGE ( 'NONE', *, *, #5237, .T. ) ;
#7111 = CIRCLE ( 'NONE', #3191, 3.224098631618459443 ) ;
#7113 = AXIS2_PLACEMENT_3D ( 'NONE', #17464, #15919, #1900 ) ;
#7114 = EDGE_LOOP ( 'NONE', ( #11369, #7169, #5626, #474 ) ) ;
#7115 = ORIENTED_EDGE ( 'NONE', *, *, #7031, .F. ) ;
#7116 = ADVANCED_FACE ( 'NONE', ( #3999 ), #10239, .T. ) ;
#7117 = VERTEX_POINT ( 'NONE', #11675 ) ;
#7118 = EDGE_CURVE ( 'NONE', #18229, #16974, #5321, .T. ) ;
#7119 = DIRECTION ( 'NONE',  ( 6.982962677686266711E-15, -0.000000000000000000, 1.000000000000000000 ) ) ;
#7120 = CARTESIAN_POINT ( 'NONE',  ( 50.93469132750264095, 59.42266395395811429, 248.9926560891072143 ) ) ;
#7121 = CARTESIAN_POINT ( 'NONE',  ( 0.000000000000000000, 0.000000000000000000, -100.0000000000000000 ) ) ;
#7122 = VERTEX_POINT ( 'NONE', #11480 ) ;
#7123 = CARTESIAN_POINT ( 'NONE',  ( -42.50000000000000000, 5.204748896376250896E-15, -49.99999999999999289 ) ) ;
#7124 = DIRECTION ( 'NONE',  ( 0.000000000000000000, 1.000000000000000000, 0.000000000000000000 ) ) ;
#7125 = CIRCLE ( 'NONE', #8100, 77.50000000000000000 ) ;
#7126 = ORIENTED_EDGE ( 'NONE', *, *, #3663, .T. ) ;
#7127 = CARTESIAN_POINT ( 'NONE',  ( 0.000000000000000000, 0.000000000000000000, 283.5832628385307999 ) ) ;
#7128 = VECTOR ( 'NONE', #18278, 999.9999999999998863 ) ;
#7129 = DIRECTION ( 'NONE',  ( 6.982962677686266711E-15, -0.000000000000000000, 1.000000000000000000 ) ) ;
#7130 = CARTESIAN_POINT ( 'NONE',  ( -7.499999999999583444, -60.00000000000000000, -105.0000000000000142 ) ) ;
#7131 = DIRECTION ( 'NONE',  ( -0.4999999999999919509, -0.8660254037844432595, 0.000000000000000000 ) ) ;
#7132 = ADVANCED_FACE ( 'NONE', ( #2287 ), #6886, .T. ) ;
#7133 = CARTESIAN_POINT ( 'NONE',  ( -134.7652707650784407, -31.41120252075685215, -19.73219286542039441 ) ) ;
#7134 = CARTESIAN_POINT ( 'NONE',  ( -73.06915264522021403, -28.06281046684251024, 248.9926560891072143 ) ) ;
#7135 = ORIENTED_EDGE ( 'NONE', *, *, #12837, .T. ) ;
#7136 = DIRECTION ( 'NONE',  ( -1.000000000000000000, 1.224646799147352961E-16, 0.000000000000000000 ) ) ;
#7137 = AXIS2_PLACEMENT_3D ( 'NONE', #19431, #5411, #19330 ) ;
#7138 = ORIENTED_EDGE ( 'NONE', *, *, #19139, .F. ) ;
#7139 = VECTOR ( 'NONE', #10420, 1000.000000000000000 ) ;
#7140 = VECTOR ( 'NONE', #2348, 1000.000000000000000 ) ;
#7141 = ORIENTED_EDGE ( 'NONE', *, *, #13616, .F. ) ;
#7142 = LINE ( 'NONE', #13361, #104 ) ;
#7143 = AXIS2_PLACEMENT_3D ( 'NONE', #13279, #19540, #8790 ) ;
#7144 = ORIENTED_EDGE ( 'NONE', *, *, #18919, .T. ) ;
#7145 = ORIENTED_EDGE ( 'NONE', *, *, #19893, .F. ) ;
#7146 = EDGE_CURVE ( 'NONE', #20213, #1969, #16302, .T. ) ;
#7147 = EDGE_CURVE ( 'NONE', #12841, #7735, #8413, .T. ) ;
#7148 = PRODUCT_RELATED_PRODUCT_CATEGORY ( 'part', '', ( #18804 ) ) ;
#7149 = CARTESIAN_POINT ( 'NONE',  ( 76.92888220842486646, -14.39940464655733976, 132.4711112102474146 ) ) ;
#7150 = CARTESIAN_POINT ( 'NONE',  ( -99.70874217756772850, -112.0725815587889969, 50.00000000000000000 ) ) ;
#7151 = DIRECTION ( 'NONE',  ( 0.000000000000000000, 0.000000000000000000, 1.000000000000000000 ) ) ;
#7152 = DIRECTION ( 'NONE',  ( 1.000000000000000000, 0.000000000000000000, 0.000000000000000000 ) ) ;
#7153 = ORIENTED_EDGE ( 'NONE', *, *, #9225, .F. ) ;
#7154 = CARTESIAN_POINT ( 'NONE',  ( -134.7540465048386977, -65.88919983460813512, 34.98379477817776007 ) ) ;
#7155 = DIRECTION ( 'NONE',  ( 1.000000000000000000, 0.000000000000000000, 0.000000000000000000 ) ) ;
#7156 = AXIS2_PLACEMENT_3D ( 'NONE', #1417, #18607, #4588 ) ;
#7157 = VECTOR ( 'NONE', #6434, 1000.000000000000000 ) ;
#7158 = DIRECTION ( 'NONE',  ( -0.000000000000000000, -0.000000000000000000, 1.000000000000000000 ) ) ;
#7159 = DIRECTION ( 'NONE',  ( -0.3088643371590125697, 0.9511061040868803440, 0.000000000000000000 ) ) ;
#7160 = VECTOR ( 'NONE', #12012, 1000.000000000000000 ) ;
#7161 = ORIENTED_EDGE ( 'NONE', *, *, #13211, .F. ) ;
#7162 = EDGE_CURVE ( 'NONE', #4103, #18829, #16397, .T. ) ;
#7163 = CARTESIAN_POINT ( 'NONE',  ( 5.693982670708940041, -0.7000608949449556029, 283.5832628385307999 ) ) ;
#7164 = FACE_OUTER_BOUND ( 'NONE', #11817, .T. ) ;
#7165 = DIRECTION ( 'NONE',  ( -0.000000000000000000, -0.000000000000000000, 1.000000000000000000 ) ) ;
#7166 = ORIENTED_EDGE ( 'NONE', *, *, #11276, .F. ) ;
#7167 = CARTESIAN_POINT ( 'NONE',  ( -71.18887634719365565, -147.8252249328922687, 60.00000000000000000 ) ) ;
#7168 = CARTESIAN_POINT ( 'NONE',  ( -77.31114765718486126, 12.23146955673674796, 132.4711112102474146 ) ) ;
#7169 = ORIENTED_EDGE ( 'NONE', *, *, #5601, .T. ) ;
#7170 = VERTEX_POINT ( 'NONE', #17732 ) ;
#7171 = AXIS2_PLACEMENT_3D ( 'NONE', #11583, #14753, #14847 ) ;
#7172 = ADVANCED_FACE ( 'NONE', ( #7183, #11580 ), #9844, .T. ) ;
#7173 = VERTEX_POINT ( 'NONE', #3709 ) ;
#7174 = VECTOR ( 'NONE', #14349, 1000.000000000000227 ) ;
#7175 = CIRCLE ( 'NONE', #15679, 79.75827554147308263 ) ;
#7176 = CARTESIAN_POINT ( 'NONE',  ( 106.6880305650188205, 105.4403344747995988, 39.99999999999999289 ) ) ;
#7177 = CARTESIAN_POINT ( 'NONE',  ( 7.950000000000000178, 0.000000000000000000, 0.000000000000000000 ) ) ;
#7178 = ORIENTED_EDGE ( 'NONE', *, *, #15408, .F. ) ;
#7179 = CARTESIAN_POINT ( 'NONE',  ( 98.08520584363758132, -113.5061255252653751, 1.878459693818897991 ) ) ;
#7180 = LINE ( 'NONE', #18213, #7333 ) ;
#7181 = EDGE_CURVE ( 'NONE', #13002, #1681, #19463, .T. ) ;
#7182 = FACE_OUTER_BOUND ( 'NONE', #1988, .T. ) ;
#7183 = FACE_OUTER_BOUND ( 'NONE', #9301, .T. ) ;
#7184 = DIRECTION ( 'NONE',  ( 1.000000000000000000, 0.000000000000000000, 0.000000000000000000 ) ) ;
#7185 = CIRCLE ( 'NONE', #5501, 106.4288957539801146 ) ;
#7186 = LINE ( 'NONE', #5850, #12821 ) ;
#7187 = AXIS2_PLACEMENT_3D ( 'NONE', #7100, #11984, #11596 ) ;
#7188 = ORIENTED_EDGE ( 'NONE', *, *, #16613, .T. ) ;
#7189 = DIRECTION ( 'NONE',  ( 1.000000000000000000, 0.000000000000000000, 0.000000000000000000 ) ) ;
#7190 = CARTESIAN_POINT ( 'NONE',  ( 135.7779226595531270, 102.2982297021113141, 60.00000000000000000 ) ) ;
#7191 = ORIENTED_EDGE ( 'NONE', *, *, #17655, .T. ) ;
#7192 = ORIENTED_EDGE ( 'NONE', *, *, #9355, .F. ) ;
#7193 = ORIENTED_EDGE ( 'NONE', *, *, #19983, .T. ) ;
#7194 = CIRCLE ( 'NONE', #15702, 15.91767397667354089 ) ;
#7195 = CARTESIAN_POINT ( 'NONE',  ( -60.47951622432784546, -49.67518383744813804, 110.7293897666001214 ) ) ;
#7196 = EDGE_LOOP ( 'NONE', ( #8090, #17108, #661, #6868 ) ) ;
#7197 = VECTOR ( 'NONE', #19845, 1000.000000000000000 ) ;
#7198 = PLANE ( 'NONE',  #18019 ) ;
#7199 = DIRECTION ( 'NONE',  ( 1.613511099790691498E-16, -1.000000000000000000, 0.000000000000000000 ) ) ;
#7200 = DIRECTION ( 'NONE',  ( 0.3420201433256694901, -0.9396926207859082059, 0.000000000000000000 ) ) ;
#7201 = ORIENTED_EDGE ( 'NONE', *, *, #6871, .F. ) ;
#7202 = DIRECTION ( 'NONE',  ( -0.2080686897406911207, -0.9781142164131917394, 0.000000000000000000 ) ) ;
#7203 = CARTESIAN_POINT ( 'NONE',  ( -34.51244174799973763, 110.9757759606085017, 39.88498244535569626 ) ) ;
#7204 = CARTESIAN_POINT ( 'NONE',  ( 134.4924637689107669, -74.66092226661579900, 6.056214776001138667 ) ) ;
#7205 = CARTESIAN_POINT ( 'NONE',  ( 0.000000000000000000, 60.00000000000000000, -105.0000000000000142 ) ) ;
#7206 = DIRECTION ( 'NONE',  ( -0.000000000000000000, -0.000000000000000000, 1.000000000000000000 ) ) ;
#7207 = CARTESIAN_POINT ( 'NONE',  ( -107.5000000000000000, -1.734524432274993541E-14, 40.00000000000000000 ) ) ;
#7208 = EDGE_LOOP ( 'NONE', ( #9848, #11862, #3715, #6867 ) ) ;
#7209 = VECTOR ( 'NONE', #8583, 1000.000000000000000 ) ;
#7210 = ORIENTED_EDGE ( 'NONE', *, *, #14652, .F. ) ;
#7211 = ORIENTED_EDGE ( 'NONE', *, *, #999, .F. ) ;
#7212 = ORIENTED_EDGE ( 'NONE', *, *, #5904, .T. ) ;
#7213 = ORIENTED_EDGE ( 'NONE', *, *, #14984, .F. ) ;
#7214 = EDGE_CURVE ( 'NONE', #9982, #13976, #17935, .T. ) ;
#7215 = VECTOR ( 'NONE', #2828, 1000.000000000000000 ) ;
#7216 = FACE_BOUND ( 'NONE', #4361, .T. ) ;
#7217 = DIRECTION ( 'NONE',  ( 0.6234898018587429203, -0.7818314824680223651, 0.000000000000000000 ) ) ;
#7218 = VERTEX_POINT ( 'NONE', #5544 ) ;
#7219 = AXIS2_PLACEMENT_3D ( 'NONE', #18452, #12199, #12408 ) ;
#7220 = CARTESIAN_POINT ( 'NONE',  ( -47.22802745636877120, -134.7565053399285091, 39.99999999999999289 ) ) ;
#7221 = DIRECTION ( 'NONE',  ( -0.000000000000000000, -1.000000000000000000, -0.000000000000000000 ) ) ;
#7222 = ORIENTED_EDGE ( 'NONE', *, *, #4894, .T. ) ;
#7223 = DIRECTION ( 'NONE',  ( 0.000000000000000000, 0.000000000000000000, 1.000000000000000000 ) ) ;
#7224 = CARTESIAN_POINT ( 'NONE',  ( 0.3563104543936381208, 9.539178283403856540, -1.477658550686872907 ) ) ;
#7225 = DIRECTION ( 'NONE',  ( -0.000000000000000000, -0.000000000000000000, -1.000000000000000000 ) ) ;
#7226 = LINE ( 'NONE', #10480, #1004 ) ;
#7227 = AXIS2_PLACEMENT_3D ( 'NONE', #12915, #6391, #16098 ) ;
#7228 = EDGE_CURVE ( 'NONE', #11511, #19487, #13104, .T. ) ;
#7229 = ADVANCED_FACE ( 'NONE', ( #2188 ), #14559, .F. ) ;
#7230 = DIRECTION ( 'NONE',  ( 0.6427876096865379196, 0.7660444431189792347, 0.000000000000000000 ) ) ;
#7231 = CYLINDRICAL_SURFACE ( 'NONE', #16232, 7.500000000000003553 ) ;
#7232 = ORIENTED_EDGE ( 'NONE', *, *, #10789, .T. ) ;
#7233 = EDGE_CURVE ( 'NONE', #7267, #19595, #8582, .T. ) ;
#7234 = DIRECTION ( 'NONE',  ( -1.000000000000000000, -5.551115123125777969E-15, 0.000000000000000000 ) ) ;
#7235 = ORIENTED_EDGE ( 'NONE', *, *, #6383, .T. ) ;
#7236 = EDGE_LOOP ( 'NONE', ( #13409, #15781, #6472, #12023 ) ) ;
#7237 = CARTESIAN_POINT ( 'NONE',  ( 0.000000000000000000, 0.000000000000000000, 132.4711112102474146 ) ) ;
#7238 = VERTEX_POINT ( 'NONE', #8707 ) ;
#7239 = ORIENTED_EDGE ( 'NONE', *, *, #18828, .T. ) ;
#7240 = EDGE_CURVE ( 'NONE', #10983, #14953, #19363, .T. ) ;
#7241 = DIRECTION ( 'NONE',  ( 0.9396926207859057634, -0.3420201433256758183, -6.456589605409169860E-15 ) ) ;
#7242 = CARTESIAN_POINT ( 'NONE',  ( -82.22461745850685588, -125.4556360547412197, 32.88769404282036390 ) ) ;
#7243 = CARTESIAN_POINT ( 'NONE',  ( 27.90514497005375461, -110.4119590718113244, 14.88498244535525750 ) ) ;
#7244 = LINE ( 'NONE', #13568, #13877 ) ;
#7245 = EDGE_LOOP ( 'NONE', ( #2994, #1504, #2360, #18314, #5439, #3600 ) ) ;
#7246 = CARTESIAN_POINT ( 'NONE',  ( -133.3341203894445357, -68.71829099011286246, 40.67712301011120246 ) ) ;
#7247 = DIRECTION ( 'NONE',  ( 1.000000000000000000, 0.000000000000000000, 0.000000000000000000 ) ) ;
#7248 = CARTESIAN_POINT ( 'NONE',  ( 1.355252715606880851E-17, 0.4400770685579600827, 9.000000000000000000 ) ) ;
#7249 = CARTESIAN_POINT ( 'NONE',  ( 75.91068486117727332, -120.9436655338208340, 39.99999999999999289 ) ) ;
#7250 = VERTEX_POINT ( 'NONE', #931 ) ;
#7251 = CIRCLE ( 'NONE', #3671, 62.91752772691707207 ) ;
#7252 = PLANE ( 'NONE',  #13950 ) ;
#7253 = EDGE_CURVE ( 'NONE', #13254, #18093, #13788, .T. ) ;
#7254 = CARTESIAN_POINT ( 'NONE',  ( -134.6687524777004796, -73.33058021821595673, 31.91433120627149123 ) ) ;
#7255 = DIRECTION ( 'NONE',  ( -0.000000000000000000, -0.000000000000000000, 1.000000000000000000 ) ) ;
#7256 = EDGE_LOOP ( 'NONE', ( #17402, #8857, #3120, #13427 ) ) ;
#7257 = ADVANCED_FACE ( 'NONE', ( #1128 ), #5745, .F. ) ;
#7258 = DIRECTION ( 'NONE',  ( -0.7430374143461878633, 0.6692498792541777819, 0.000000000000000000 ) ) ;
#7259 = DIRECTION ( 'NONE',  ( -0.000000000000000000, -0.000000000000000000, 1.000000000000000000 ) ) ;
#7260 = ORIENTED_EDGE ( 'NONE', *, *, #17492, .T. ) ;
#7261 = ORIENTED_EDGE ( 'NONE', *, *, #4068, .T. ) ;
#7262 = CARTESIAN_POINT ( 'NONE',  ( -97.49999999993794120, -115.4778303847070902, 29.92289092923461524 ) ) ;
#7263 = FACE_OUTER_BOUND ( 'NONE', #16751, .T. ) ;
#7264 = ADVANCED_FACE ( 'NONE', ( #12379 ), #19849, .T. ) ;
#7265 = DIRECTION ( 'NONE',  ( 0.000000000000000000, 0.000000000000000000, 1.000000000000000000 ) ) ;
#7266 = VECTOR ( 'NONE', #2812, 1000.000000000000000 ) ;
#7267 = VERTEX_POINT ( 'NONE', #12062 ) ;
#7268 = LINE ( 'NONE', #8896, #4435 ) ;
#7269 = DIRECTION ( 'NONE',  ( 0.000000000000000000, 0.000000000000000000, -1.000000000000000000 ) ) ;
#7270 = CARTESIAN_POINT ( 'NONE',  ( -136.4994460260996902, -31.11111111111111072, -9.999999999999985789 ) ) ;
#7271 = PLANE ( 'NONE',  #12094 ) ;
#7272 = DIRECTION ( 'NONE',  ( -0.5000000000000009992, 0.8660254037844380415, 0.000000000000000000 ) ) ;
#7273 = DIRECTION ( 'NONE',  ( 1.000000000000000000, 0.000000000000000000, 0.000000000000000000 ) ) ;
#7274 = EDGE_CURVE ( 'NONE', #8089, #4188, #3990, .T. ) ;
#7275 = DIRECTION ( 'NONE',  ( -6.982962677686266711E-15, 0.000000000000000000, -1.000000000000000000 ) ) ;
#7276 = FACE_OUTER_BOUND ( 'NONE', #3453, .T. ) ;
#7277 = LINE ( 'NONE', #18125, #6312 ) ;
#7278 = ADVANCED_FACE ( 'NONE', ( #9105 ), #4509, .F. ) ;
#7279 = ORIENTED_EDGE ( 'NONE', *, *, #13842, .T. ) ;
#7280 = CARTESIAN_POINT ( 'NONE',  ( 7.948937137877743808, -60.22232964560488000, 293.5832628385307999 ) ) ;
#7281 = DIRECTION ( 'NONE',  ( -0.000000000000000000, -0.000000000000000000, -1.000000000000000000 ) ) ;
#7282 = AXIS2_PLACEMENT_3D ( 'NONE', #17718, #7259, #13480 ) ;
#7283 = ORIENTED_EDGE ( 'NONE', *, *, #15557, .F. ) ;
#7284 = ADVANCED_FACE ( 'NONE', ( #5847 ), #7469, .F. ) ;
#7285 = EDGE_LOOP ( 'NONE', ( #594, #10961, #7413 ) ) ;
#7286 = EDGE_CURVE ( 'NONE', #6626, #2011, #13499, .T. ) ;
#7287 = AXIS2_PLACEMENT_3D ( 'NONE', #5704, #10592, #13560 ) ;
#7288 = ORIENTED_EDGE ( 'NONE', *, *, #18109, .T. ) ;
#7289 = CARTESIAN_POINT ( 'NONE',  ( -110.0000000000000142, 265.0000000000000000, 5.000000000000000888 ) ) ;
#7290 = VERTEX_POINT ( 'NONE', #19950 ) ;
#7291 = DIRECTION ( 'NONE',  ( 0.3420201433256662704, 0.9396926207859092051, 0.000000000000000000 ) ) ;
#7292 = LINE ( 'NONE', #13727, #15965 ) ;
#7293 = DIRECTION ( 'NONE',  ( -0.000000000000000000, -0.000000000000000000, 1.000000000000000000 ) ) ;
#7294 = ORIENTED_EDGE ( 'NONE', *, *, #2975, .T. ) ;
#7295 = CYLINDRICAL_SURFACE ( 'NONE', #19263, 9.999999999999994671 ) ;
#7296 = CARTESIAN_POINT ( 'NONE',  ( -130.0656023054207822, -74.72982709287477121, -6.442063508531142624 ) ) ;
#7297 = CARTESIAN_POINT ( 'NONE',  ( 122.8001410695374460, -86.14014948502070013, 8.673617379884035472E-15 ) ) ;
#7298 = CIRCLE ( 'NONE', #11553, 3.224098631618458999 ) ;
#7299 = CARTESIAN_POINT ( 'NONE',  ( 0.000000000000000000, 0.000000000000000000, 293.5832628385307999 ) ) ;
#7300 = CARTESIAN_POINT ( 'NONE',  ( 0.000000000000000000, 0.000000000000000000, 283.5832628385307999 ) ) ;
#7301 = DIRECTION ( 'NONE',  ( -0.000000000000000000, -0.000000000000000000, 1.000000000000000000 ) ) ;
#7302 = ORIENTED_EDGE ( 'NONE', *, *, #19446, .F. ) ;
#7303 = DIRECTION ( 'NONE',  ( 0.000000000000000000, 1.000000000000000000, 0.000000000000000000 ) ) ;
#7304 = PRESENTATION_LAYER_ASSIGNMENT (  '', '', ( #13493 ) ) ;
#7305 = EDGE_LOOP ( 'NONE', ( #16444, #9480, #14567, #14590 ) ) ;
#7306 = ORIENTED_EDGE ( 'NONE', *, *, #16109, .F. ) ;
#7307 = ORIENTED_EDGE ( 'NONE', *, *, #1870, .T. ) ;
#7308 = ORIENTED_EDGE ( 'NONE', *, *, #19114, .F. ) ;
#7309 = CIRCLE ( 'NONE', #17457, 60.74260934110282051 ) ;
#7310 = PLANE ( 'NONE',  #1784 ) ;
#7311 = AXIS2_PLACEMENT_3D ( 'NONE', #481, #14788, #19309 ) ;
#7312 = CARTESIAN_POINT ( 'NONE',  ( 10.52001906124917774, 3.255534882826434551, 248.9926560891072143 ) ) ;
#7313 = ORIENTED_EDGE ( 'NONE', *, *, #13994, .T. ) ;
#7314 = CARTESIAN_POINT ( 'NONE',  ( 0.000000000000000000, 0.000000000000000000, 49.99999999999999289 ) ) ;
#7315 = CARTESIAN_POINT ( 'NONE',  ( -57.94128254008190027, -9.381844291199545438, 112.0427633081291816 ) ) ;
#7316 = ORIENTED_EDGE ( 'NONE', *, *, #7762, .F. ) ;
#7317 = CARTESIAN_POINT ( 'NONE',  ( 130.9868171408399746, -91.88282611735537841, 40.00000000000000000 ) ) ;
#7318 = CARTESIAN_POINT ( 'NONE',  ( -20.21777810286715749, -59.58067424803620327, 293.5832628385307999 ) ) ;
#7319 = CARTESIAN_POINT ( 'NONE',  ( -131.4992782843381462, -89.99675518205303604, 0.04849131325310787610 ) ) ;
#7320 = DIRECTION ( 'NONE',  ( 1.000000000000000000, 0.000000000000000000, 0.000000000000000000 ) ) ;
#7321 = CARTESIAN_POINT ( 'NONE',  ( 127.6186898578139761, -78.88112642940112096, 40.77662057728262113 ) ) ;
#7322 = AXIS2_PLACEMENT_3D ( 'NONE', #18005, #16274, #3973 ) ;
#7323 = DIRECTION ( 'NONE',  ( -0.6155349844899689060, 0.7881095627315620744, 0.000000000000000000 ) ) ;
#7324 = ORIENTED_EDGE ( 'NONE', *, *, #17180, .F. ) ;
#7325 = ADVANCED_FACE ( 'NONE', ( #13708, #18326, #15243, #5951, #4301, #4202 ), #10432, .T. ) ;
#7326 = CARTESIAN_POINT ( 'NONE',  ( -176.7850001792985211, -188.8278678429259685, 32.32637774726087798 ) ) ;
#7327 = AXIS2_PLACEMENT_3D ( 'NONE', #1359, #7586, #7490 ) ;
#7328 = ORIENTED_EDGE ( 'NONE', *, *, #10236, .T. ) ;
#7329 = ORIENTED_EDGE ( 'NONE', *, *, #525, .F. ) ;
#7330 = DIRECTION ( 'NONE',  ( 1.000000000000000000, 0.000000000000000000, 0.000000000000000000 ) ) ;
#7331 = VERTEX_POINT ( 'NONE', #2676 ) ;
#7332 = VERTEX_POINT ( 'NONE', #8900 ) ;
#7333 = VECTOR ( 'NONE', #8897, 1000.000000000000000 ) ;
#7334 = DIRECTION ( 'NONE',  ( -1.000000000000000000, 0.000000000000000000, 0.000000000000000000 ) ) ;
#7335 = ADVANCED_FACE ( 'NONE', ( #18430 ), #1340, .T. ) ;
#7336 = CARTESIAN_POINT ( 'NONE',  ( 0.000000000000000000, 0.000000000000000000, 293.5832628385307999 ) ) ;
#7337 = ORIENTED_EDGE ( 'NONE', *, *, #18532, .F. ) ;
#7338 = VECTOR ( 'NONE', #10922, 1000.000000000000000 ) ;
#7339 = FACE_BOUND ( 'NONE', #12467, .T. ) ;
#7340 = DIRECTION ( 'NONE',  ( -0.5300553768524375320, -0.8479630283625697595, 0.000000000000000000 ) ) ;
#7341 = EDGE_CURVE ( 'NONE', #13125, #1887, #12487, .T. ) ;
#7342 = VERTEX_POINT ( 'NONE', #16788 ) ;
#7343 = DIRECTION ( 'NONE',  ( 1.000000000000000000, 0.000000000000000000, 0.000000000000000000 ) ) ;
#7344 = CARTESIAN_POINT ( 'NONE',  ( 19.23677882349201695, -57.61823435390814296, 293.5832628385307999 ) ) ;
#7345 = CYLINDRICAL_SURFACE ( 'NONE', #18459, 7.500000000000007105 ) ;
#7346 = ORIENTED_EDGE ( 'NONE', *, *, #5226, .F. ) ;
#7347 = CARTESIAN_POINT ( 'NONE',  ( 71.18887634719571622, -147.8252249328912740, 49.99999999999999289 ) ) ;
#7348 = CARTESIAN_POINT ( 'NONE',  ( -71.18887634719365565, -147.8252249328922687, 39.99999999999999289 ) ) ;
#7349 = VECTOR ( 'NONE', #14012, 1000.000000000000000 ) ;
#7350 = CARTESIAN_POINT ( 'NONE',  ( -71.18887634719365565, -147.8252249328922687, 60.00000000000000000 ) ) ;
#7351 = ORIENTED_EDGE ( 'NONE', *, *, #19509, .F. ) ;
#7352 = EDGE_CURVE ( 'NONE', #12362, #6494, #5977, .T. ) ;
#7353 = CYLINDRICAL_SURFACE ( 'NONE', #12013, 140.0000000000000284 ) ;
#7354 = DIRECTION ( 'NONE',  ( -0.7660444431189770143, 0.6427876096865404731, 5.348151281215661977E-15 ) ) ;
#7355 = ORIENTED_EDGE ( 'NONE', *, *, #1328, .F. ) ;
#7356 = EDGE_LOOP ( 'NONE', ( #7346, #12000, #10954, #4513 ) ) ;
#7357 = CARTESIAN_POINT ( 'NONE',  ( -107.4999999999999858, -118.5063289449133777, 40.00000000000000000 ) ) ;
#7358 = EDGE_LOOP ( 'NONE', ( #4462, #14287, #6636, #17081 ) ) ;
#7359 = AXIS2_PLACEMENT_3D ( 'NONE', #2734, #7529, #9168 ) ;
#7360 = DIRECTION ( 'NONE',  ( -1.000000000000000000, 0.000000000000000000, 0.000000000000000000 ) ) ;
#7361 = EDGE_CURVE ( 'NONE', #4545, #1924, #7568, .T. ) ;
#7362 = CARTESIAN_POINT ( 'NONE',  ( -56.50138340076688337, 22.29928840491054487, 283.5832628385307999 ) ) ;
#7363 = VERTEX_POINT ( 'NONE', #18526 ) ;
#7364 = CARTESIAN_POINT ( 'NONE',  ( 96.81625497255032542, -114.6298681929799557, 3.428784747764392460 ) ) ;
#7365 = LINE ( 'NONE', #10734, #5754 ) ;
#7366 = EDGE_CURVE ( 'NONE', #2014, #13413, #16995, .T. ) ;
#7367 = DIRECTION ( 'NONE',  ( -0.1736481776669273613, 0.9848077530122085754, 1.238751781085795780E-15 ) ) ;
#7368 = CARTESIAN_POINT ( 'NONE',  ( -109.9999999999983515, 275.0000000000000000, 77.50000000000000000 ) ) ;
#7369 = DIRECTION ( 'NONE',  ( 6.982962677686266711E-15, -0.000000000000000000, 1.000000000000000000 ) ) ;
#7370 = CYLINDRICAL_SURFACE ( 'NONE', #16249, 60.74260934110282051 ) ;
#7371 = PLANE ( 'NONE',  #20215 ) ;
#7372 = FACE_OUTER_BOUND ( 'NONE', #3399, .T. ) ;
#7373 = ORIENTED_EDGE ( 'NONE', *, *, #18850, .T. ) ;
#7374 = ADVANCED_FACE ( 'NONE', ( #1444 ), #20159, .F. ) ;
#7375 = DIRECTION ( 'NONE',  ( -0.9993852124581887875, 0.03505990758545896036, 0.000000000000000000 ) ) ;
#7376 = CARTESIAN_POINT ( 'NONE',  ( 32.03743494504719536, 36.03492788066214558, 248.9926560891072143 ) ) ;
#7377 = ORIENTED_EDGE ( 'NONE', *, *, #1855, .F. ) ;
#7378 = VECTOR ( 'NONE', #11119, 999.9999999999998863 ) ;
#7379 = VERTEX_POINT ( 'NONE', #15870 ) ;
#7380 = ORIENTED_EDGE ( 'NONE', *, *, #13442, .F. ) ;
#7381 = CARTESIAN_POINT ( 'NONE',  ( 60.68567895461851691, -2.629250726500488078, 283.5832628385307999 ) ) ;
#7382 = ORIENTED_EDGE ( 'NONE', *, *, #11875, .T. ) ;
#7383 = EDGE_CURVE ( 'NONE', #6649, #14876, #15561, .T. ) ;
#7384 = DIRECTION ( 'NONE',  ( 1.000000000000000000, 0.000000000000000000, 0.000000000000000000 ) ) ;
#7385 = VECTOR ( 'NONE', #35, 1000.000000000000000 ) ;
#7386 = EDGE_CURVE ( 'NONE', #13644, #8891, #5635, .T. ) ;
#7387 = ADVANCED_FACE ( 'NONE', ( #1848 ), #6668, .F. ) ;
#7388 = CLOSED_SHELL ( 'NONE', ( #11718, #16256, #18901, #373, #9034, #19166, #15927, #14415, #17648, #15605, #19262, #10516, #4981, #16900 ) ) ;
#7389 = LINE ( 'NONE', #2691, #695 ) ;
#7390 = DIRECTION ( 'NONE',  ( -0.000000000000000000, -0.000000000000000000, 1.000000000000000000 ) ) ;
#7391 = CARTESIAN_POINT ( 'NONE',  ( 32.61983739937762294, 51.24071425735590424, 293.5832628385307999 ) ) ;
#7392 = VERTEX_POINT ( 'NONE', #8079 ) ;
#7393 = DIRECTION ( 'NONE',  ( 0.000000000000000000, 0.000000000000000000, -1.000000000000000000 ) ) ;
#7394 = CARTESIAN_POINT ( 'NONE',  ( -131.4393841463108288, -72.38802639018405216, 2.524901613696201697 ) ) ;
#7395 = CARTESIAN_POINT ( 'NONE',  ( 131.2164711380734730, -72.78471332658568826, 2.208503663874919365 ) ) ;
#7396 = CYLINDRICAL_SURFACE ( 'NONE', #358, 10.00000000000000888 ) ;
#7397 = LINE ( 'NONE', #9032, #12975 ) ;
#7398 = CARTESIAN_POINT ( 'NONE',  ( -60.00000000000000000, -2.094888803305880013E-13, -105.0000000000000142 ) ) ;
#7399 = EDGE_CURVE ( 'NONE', #8543, #14775, #11, .T. ) ;
#7400 = ORIENTED_EDGE ( 'NONE', *, *, #11357, .T. ) ;
#7401 = CARTESIAN_POINT ( 'NONE',  ( 7.950000000000000178, 10.39230484541327471, -5.498853076140229456E-16 ) ) ;
#7402 = VECTOR ( 'NONE', #10919, 1000.000000000000114 ) ;
#7403 = VERTEX_POINT ( 'NONE', #109 ) ;
#7404 = VECTOR ( 'NONE', #4949, 1000.000000000000000 ) ;
#7405 = VERTEX_POINT ( 'NONE', #3388 ) ;
#7406 = VERTEX_POINT ( 'NONE', #11049 ) ;
#7407 = CIRCLE ( 'NONE', #18868, 62.91752772691707207 ) ;
#7408 = ORIENTED_EDGE ( 'NONE', *, *, #14389, .T. ) ;
#7409 = EDGE_CURVE ( 'NONE', #8342, #17256, #15668, .T. ) ;
#7410 = CARTESIAN_POINT ( 'NONE',  ( -110.0000000000000142, 1.347111479062088839E-14, -9.999999999999994671 ) ) ;
#7411 = CARTESIAN_POINT ( 'NONE',  ( 15.91767397667354800, 164.0736214083062805, 49.99999999999999289 ) ) ;
#7412 = FACE_OUTER_BOUND ( 'NONE', #4357, .T. ) ;
#7413 = ORIENTED_EDGE ( 'NONE', *, *, #5601, .F. ) ;
#7414 = DIRECTION ( 'NONE',  ( 1.000000000000000000, 0.000000000000000000, 0.000000000000000000 ) ) ;
#7415 = FACE_OUTER_BOUND ( 'NONE', #16101, .T. ) ;
#7416 = ADVANCED_FACE ( 'NONE', ( #9423 ), #18842, .F. ) ;
#7417 = ORIENTED_EDGE ( 'NONE', *, *, #17876, .T. ) ;
#7418 = CARTESIAN_POINT ( 'NONE',  ( -82.11169388575343930, 112.6076301679229772, -16.15456432045361979 ) ) ;
#7419 = LINE ( 'NONE', #9159, #2353 ) ;
#7420 = CARTESIAN_POINT ( 'NONE',  ( 128.2779226595531270, 102.2982297021113141, 60.00000000000000000 ) ) ;
#7421 = CARTESIAN_POINT ( 'NONE',  ( 37.78198917157319414, -47.56244194535178593, 293.5832628385307999 ) ) ;
#7422 = AXIS2_PLACEMENT_3D ( 'NONE', #2593, #18236, #16806 ) ;
#7423 = CIRCLE ( 'NONE', #18206, 7.500000000000007105 ) ;
#7424 = UNCERTAINTY_MEASURE_WITH_UNIT (LENGTH_MEASURE( 1.000000000000000082E-05 ), #13400, 'distance_accuracy_value', 'NONE');
#7425 = CARTESIAN_POINT ( 'NONE',  ( 15.91767397667354800, 164.0736214083062805, 60.00000000000000000 ) ) ;
#7426 = LINE ( 'NONE', #18477, #20132 ) ;
#7427 = VERTEX_POINT ( 'NONE', #3288 ) ;
#7428 = DIRECTION ( 'NONE',  ( 0.000000000000000000, 0.000000000000000000, 1.000000000000000000 ) ) ;
#7429 = VERTEX_POINT ( 'NONE', #17204 ) ;
#7430 = VERTEX_POINT ( 'NONE', #5033 ) ;
#7431 = CARTESIAN_POINT ( 'NONE',  ( 39.37628763770420193, 49.07263256785965666, 132.4711112102474146 ) ) ;
#7432 = ORIENTED_EDGE ( 'NONE', *, *, #19795, .T. ) ;
#7433 = EDGE_LOOP ( 'NONE', ( #13634, #19564, #128, #14785 ) ) ;
#7434 = CIRCLE ( 'NONE', #18563, 15.91767397667354089 ) ;
#7435 = DIRECTION ( 'NONE',  ( 0.4999999999999950040, 0.8660254037844415942, 0.000000000000000000 ) ) ;
#7436 = CARTESIAN_POINT ( 'NONE',  ( 0.000000000000000000, 0.000000000000000000, 293.5832628385307999 ) ) ;
#7437 = DIRECTION ( 'NONE',  ( -0.000000000000000000, -1.000000000000000000, -0.000000000000000000 ) ) ;
#7438 = EDGE_LOOP ( 'NONE', ( #310, #7787, #5093, #15364 ) ) ;
#7439 = LINE ( 'NONE', #1621, #16532 ) ;
#7440 = DIRECTION ( 'NONE',  ( 1.000000000000000000, 0.000000000000000000, 0.000000000000000000 ) ) ;
#7441 = ORIENTED_EDGE ( 'NONE', *, *, #11168, .T. ) ;
#7442 = CARTESIAN_POINT ( 'NONE',  ( -88.53631457789035153, 115.2621388628904526, -28.80465452976635632 ) ) ;
#7443 = CARTESIAN_POINT ( 'NONE',  ( -163.5019688434124419, -20.99123081650240863, 49.99999999999999289 ) ) ;
#7444 = DIRECTION ( 'NONE',  ( -0.9848077530122097967, 0.1736481776669206722, 0.000000000000000000 ) ) ;
#7445 = DIRECTION ( 'NONE',  ( 0.000000000000000000, 0.000000000000000000, -1.000000000000000000 ) ) ;
#7446 = CYLINDRICAL_SURFACE ( 'NONE', #13381, 15.91767397667354800 ) ;
#7447 = DIRECTION ( 'NONE',  ( -0.000000000000000000, -0.000000000000000000, 1.000000000000000000 ) ) ;
#7448 = VECTOR ( 'NONE', #10162, 1000.000000000000114 ) ;
#7449 = ORIENTED_EDGE ( 'NONE', *, *, #18275, .T. ) ;
#7450 = AXIS2_PLACEMENT_3D ( 'NONE', #8081, #12581, #6265 ) ;
#7451 = VECTOR ( 'NONE', #9007, 1000.000000000000000 ) ;
#7452 = FACE_BOUND ( 'NONE', #7583, .T. ) ;
#7453 = CARTESIAN_POINT ( 'NONE',  ( -12.16118437606760949, -23.99289710269258080, 39.88498244535554704 ) ) ;
#7454 = VERTEX_POINT ( 'NONE', #9317 ) ;
#7455 = EDGE_LOOP ( 'NONE', ( #3013, #16994, #17891, #8761 ) ) ;
#7456 = CARTESIAN_POINT ( 'NONE',  ( -82.03125000005908873, -125.5821405432628382, 30.74521087840624034 ) ) ;
#7457 = ORIENTED_EDGE ( 'NONE', *, *, #19302, .F. ) ;
#7458 = DIRECTION ( 'NONE',  ( 0.5000000000000039968, 0.8660254037844362651, -3.488592933436653225E-15 ) ) ;
#7459 = LINE ( 'NONE', #13802, #12854 ) ;
#7460 = ORIENTED_EDGE ( 'NONE', *, *, #7736, .T. ) ;
#7461 = AXIS2_PLACEMENT_3D ( 'NONE', #15313, #9283, #14193 ) ;
#7462 = CARTESIAN_POINT ( 'NONE',  ( 99.98863955314980956, -130.5690324404832268, 3.390001990510095986 ) ) ;
#7463 = PLANE ( 'NONE',  #161 ) ;
#7464 = VECTOR ( 'NONE', #14960, 1000.000000000000114 ) ;
#7465 = VECTOR ( 'NONE', #12192, 1000.000000000000000 ) ;
#7466 = EDGE_CURVE ( 'NONE', #6324, #12822, #4990, .T. ) ;
#7467 = CARTESIAN_POINT ( 'NONE',  ( -137.2265357449624616, -24.54992354075934458, -16.95325888733908215 ) ) ;
#7468 = SURFACE_STYLE_USAGE ( .BOTH. , #107 ) ;
#7469 = CYLINDRICAL_SURFACE ( 'NONE', #14784, 106.4288957539800862 ) ;
#7470 = CARTESIAN_POINT ( 'NONE',  ( 0.3552109633508171438, -3.484997970623485930, 8.999999999999998224 ) ) ;
#7471 = DIRECTION ( 'NONE',  ( 0.9396926207859082059, 0.3420201433256694901, 0.000000000000000000 ) ) ;
#7472 = CARTESIAN_POINT ( 'NONE',  ( 95.77047472624727220, -116.1200526047208967, 30.77282038149522236 ) ) ;
#7473 = ORIENTED_EDGE ( 'NONE', *, *, #3002, .F. ) ;
#7474 = ADVANCED_FACE ( 'NONE', ( #1547 ), #17411, .F. ) ;
#7475 = PLANE ( 'NONE',  #18896 ) ;
#7476 = DIRECTION ( 'NONE',  ( -0.000000000000000000, -0.000000000000000000, 1.000000000000000000 ) ) ;
#7477 = EDGE_CURVE ( 'NONE', #17480, #17433, #18638, .T. ) ;
#7478 = ORIENTED_EDGE ( 'NONE', *, *, #3119, .F. ) ;
#7479 = VECTOR ( 'NONE', #10479, 999.9999999999998863 ) ;
#7480 = CIRCLE ( 'NONE', #11405, 62.91752772691707207 ) ;
#7481 = ADVANCED_FACE ( 'NONE', ( #11254 ), #9524, .F. ) ;
#7482 = ORIENTED_EDGE ( 'NONE', *, *, #14262, .T. ) ;
#7483 = ORIENTED_EDGE ( 'NONE', *, *, #84, .F. ) ;
#7484 = FACE_BOUND ( 'NONE', #5885, .T. ) ;
#7485 = ORIENTED_EDGE ( 'NONE', *, *, #5783, .T. ) ;
#7486 = PLANE ( 'NONE',  #10870 ) ;
#7487 = CARTESIAN_POINT ( 'NONE',  ( 134.7188131032333445, -72.93593548660993520, 10.00000000000000178 ) ) ;
#7488 = DIRECTION ( 'NONE',  ( -0.000000000000000000, -0.000000000000000000, 1.000000000000000000 ) ) ;
#7489 = EDGE_CURVE ( 'NONE', #3695, #16332, #4615, .T. ) ;
#7490 = DIRECTION ( 'NONE',  ( 1.000000000000000000, 0.000000000000000000, -0.000000000000000000 ) ) ;
#7491 = DIRECTION ( 'NONE',  ( 0.8186676071302493307, -0.5742676632334713371, 0.000000000000000000 ) ) ;
#7492 = CARTESIAN_POINT ( 'NONE',  ( 107.5000000000000000, 1.734524432274993541E-14, 30.00000000000000000 ) ) ;
#7493 = VECTOR ( 'NONE', #16681, 1000.000000000000000 ) ;
#7494 = CIRCLE ( 'NONE', #16646, 62.91752772691707207 ) ;
#7495 = VERTEX_POINT ( 'NONE', #7880 ) ;
#7496 = CARTESIAN_POINT ( 'NONE',  ( 1.379293853801755176, 62.91752772691707207, 248.9926560891072143 ) ) ;
#7497 = FACE_OUTER_BOUND ( 'NONE', #10882, .T. ) ;
#7498 = CARTESIAN_POINT ( 'NONE',  ( 134.0015816819113184, -77.97298368086231335, 3.467253640805495252 ) ) ;
#7499 = FACE_OUTER_BOUND ( 'NONE', #13075, .T. ) ;
#7500 = CARTESIAN_POINT ( 'NONE',  ( -40.27908801169994035, -45.46712722958821473, 283.5832628385307999 ) ) ;
#7501 = FACE_OUTER_BOUND ( 'NONE', #7236, .T. ) ;
#7502 = ORIENTED_EDGE ( 'NONE', *, *, #4969, .T. ) ;
#7503 = DIRECTION ( 'NONE',  ( -0.000000000000000000, -0.000000000000000000, 1.000000000000000000 ) ) ;
#7504 = EDGE_CURVE ( 'NONE', #7430, #3408, #311, .T. ) ;
#7505 = EDGE_CURVE ( 'NONE', #9853, #5389, #206, .T. ) ;
#7506 = ORIENTED_EDGE ( 'NONE', *, *, #6398, .T. ) ;
#7507 = VECTOR ( 'NONE', #19360, 1000.000000000000000 ) ;
#7508 = VERTEX_POINT ( 'NONE', #12686 ) ;
#7509 = VERTEX_POINT ( 'NONE', #18950 ) ;
#7510 = LINE ( 'NONE', #966, #9600 ) ;
#7511 = EDGE_CURVE ( 'NONE', #17939, #7290, #4935, .T. ) ;
#7512 = DIRECTION ( 'NONE',  ( -1.000000000000000000, 0.000000000000000000, -0.000000000000000000 ) ) ;
#7513 = DIRECTION ( 'NONE',  ( -0.3420201433256694901, 0.9396926207859082059, 0.000000000000000000 ) ) ;
#7514 = VERTEX_POINT ( 'NONE', #2061 ) ;
#7515 = CARTESIAN_POINT ( 'NONE',  ( 7.350000000000001421, 0.000000000000000000, 0.000000000000000000 ) ) ;
#7516 = LINE ( 'NONE', #6406, #8481 ) ;
#7517 = ORIENTED_EDGE ( 'NONE', *, *, #6258, .F. ) ;
#7518 = CARTESIAN_POINT ( 'NONE',  ( -78.37722339831623231, 116.0043570404596522, -9.999999999999984013 ) ) ;
#7519 = CARTESIAN_POINT ( 'NONE',  ( 0.07661102881317853608, 8.673996836102551455, -2.976196775178697962 ) ) ;
#7520 = DIRECTION ( 'NONE',  ( -1.000000000000000000, 0.000000000000000000, 0.000000000000000000 ) ) ;
#7521 = PRODUCT_DEFINITION_FORMATION_WITH_SPECIFIED_SOURCE ( 'ANY', '', #9652, .NOT_KNOWN. ) ;
#7522 = AXIS2_PLACEMENT_3D ( 'NONE', #4072, #10307, #8782 ) ;
#7523 = CARTESIAN_POINT ( 'NONE',  ( -17.24542129382122724, 20.55229278271246329, 14.88498244535557369 ) ) ;
#7524 = EDGE_CURVE ( 'NONE', #934, #93, #14824, .T. ) ;
#7525 = CARTESIAN_POINT ( 'NONE',  ( -189.9999999999988916, 285.0000000000000568, -2.499999999999734879 ) ) ;
#7526 = DIRECTION ( 'NONE',  ( 0.000000000000000000, 0.000000000000000000, 1.000000000000000000 ) ) ;
#7527 = ORIENTED_EDGE ( 'NONE', *, *, #3413, .F. ) ;
#7528 = VERTEX_POINT ( 'NONE', #8489 ) ;
#7529 = DIRECTION ( 'NONE',  ( -0.000000000000000000, -0.000000000000000000, 1.000000000000000000 ) ) ;
#7530 = ORIENTED_EDGE ( 'NONE', *, *, #18776, .T. ) ;
#7531 = EDGE_CURVE ( 'NONE', #7429, #16671, #9880, .T. ) ;
#7532 = ORIENTED_EDGE ( 'NONE', *, *, #1371, .T. ) ;
#7533 = CYLINDRICAL_SURFACE ( 'NONE', #6648, 60.74260934110282051 ) ;
#7534 = CIRCLE ( 'NONE', #15056, 62.91752772691707207 ) ;
#7535 = ORIENTED_EDGE ( 'NONE', *, *, #904, .F. ) ;
#7536 = EDGE_LOOP ( 'NONE', ( #8993, #20092 ) ) ;
#7537 = CIRCLE ( 'NONE', #8203, 7.500000000000001776 ) ;
#7538 = FACE_OUTER_BOUND ( 'NONE', #3341, .T. ) ;
#7539 =( NAMED_UNIT ( * ) SI_UNIT ( $, .STERADIAN. ) SOLID_ANGLE_UNIT ( ) );
#7540 = CARTESIAN_POINT ( 'NONE',  ( 1.396592535537253342E-14, 0.000000000000000000, 60.00000000000000000 ) ) ;
#7541 = ORIENTED_EDGE ( 'NONE', *, *, #16801, .F. ) ;
#7542 = CARTESIAN_POINT ( 'NONE',  ( 15.91767397667354089, 149.1530343478547422, 60.00000000000000000 ) ) ;
#7543 = CARTESIAN_POINT ( 'NONE',  ( -29.99999999999887379, 275.0000000000000000, 4.999999999999158007 ) ) ;
#7544 = ORIENTED_EDGE ( 'NONE', *, *, #5640, .T. ) ;
#7545 = LINE ( 'NONE', #12246, #8702 ) ;
#7546 = CARTESIAN_POINT ( 'NONE',  ( 0.000000000000000000, 0.000000000000000000, 293.5832628385307999 ) ) ;
#7547 = DIRECTION ( 'NONE',  ( 1.000000000000000000, 0.000000000000000000, 0.000000000000000000 ) ) ;
#7548 = VECTOR ( 'NONE', #14622, 1000.000000000000000 ) ;
#7549 = CYLINDRICAL_SURFACE ( 'NONE', #18879, 60.74260934110282051 ) ;
#7550 = DIRECTION ( 'NONE',  ( -0.8479630283625716469, 0.5300553768524345344, 0.000000000000000000 ) ) ;
#7551 = LINE ( 'NONE', #6341, #13251 ) ;
#7552 = ORIENTED_EDGE ( 'NONE', *, *, #12778, .F. ) ;
#7553 = B_SPLINE_CURVE_WITH_KNOTS ( 'NONE', 3,
 ( #134, #18866, #38, #4852, #4746, #18765, #3209, #19167, #17337, #11383, #17539, #10970, #14453, #15993, #11280, #17229, #9447, #3414, #440, #1981, #9644, #3313, #6289, #19073, #8207, #14252 ),
 .UNSPECIFIED., .F., .F.,
 ( 4, 2, 2, 2, 2, 2, 2, 2, 2, 2, 2, 2, 4 ),
 ( 6.938893903907228378E-18, 0.005933429007670090738, 0.01186685801534017454, 0.02373371603068033520, 0.02966714503835042246, 0.03560057404602051667, 0.04746743206136066345, 0.05933429007670083105, 0.07120114809204097783, 0.07416786259587601626, 0.07713457709971105469, 0.08306800610738104829, 0.09493486412272097996 ),
 .UNSPECIFIED. ) ;
#7554 = CARTESIAN_POINT ( 'NONE',  ( 82.03125000000004263, -125.5821405433013780, 30.00000000000000000 ) ) ;
#7555 = FACE_OUTER_BOUND ( 'NONE', #7356, .T. ) ;
#7556 = VERTEX_POINT ( 'NONE', #19441 ) ;
#7557 = ORIENTED_EDGE ( 'NONE', *, *, #14156, .F. ) ;
#7558 = SHAPE_REPRESENTATION ( 'Back Cover', ( #18639 ), #12 ) ;
#7559 = PLANE ( 'NONE',  #1591 ) ;
#7560 = ORIENTED_EDGE ( 'NONE', *, *, #15369, .F. ) ;
#7561 = CARTESIAN_POINT ( 'NONE',  ( -144.0985391606959354, 40.21647770819863865, -15.98578004590384438 ) ) ;
#7562 = DIRECTION ( 'NONE',  ( 1.000000000000000000, 0.000000000000000000, 0.000000000000000000 ) ) ;
#7563 = ORIENTED_EDGE ( 'NONE', *, *, #9079, .F. ) ;
#7564 = CARTESIAN_POINT ( 'NONE',  ( 96.95682486763449504, -115.7027609143983398, 10.38738059575018724 ) ) ;
#7565 = DIRECTION ( 'NONE',  ( 1.000000000000000000, 0.000000000000000000, 0.000000000000000000 ) ) ;
#7566 = VECTOR ( 'NONE', #5181, 1000.000000000000114 ) ;
#7567 = LINE ( 'NONE', #18324, #7197 ) ;
#7568 = LINE ( 'NONE', #13811, #20011 ) ;
#7569 = CARTESIAN_POINT ( 'NONE',  ( 0.000000000000000000, 0.000000000000000000, 60.00000000000000000 ) ) ;
#7570 = DIRECTION ( 'NONE',  ( 1.000000000000000000, 0.000000000000000000, -0.000000000000000000 ) ) ;
#7571 = CARTESIAN_POINT ( 'NONE',  ( 100.4426743476961974, -129.9257371803372791, 37.11542010922146062 ) ) ;
#7572 = ORIENTED_EDGE ( 'NONE', *, *, #17307, .T. ) ;
#7573 = CARTESIAN_POINT ( 'NONE',  ( -110.0000000000000142, 275.0000000000000000, -82.50000000000001421 ) ) ;
#7574 = LINE ( 'NONE', #7376, #6640 ) ;
#7575 = ORIENTED_EDGE ( 'NONE', *, *, #5367, .F. ) ;
#7576 = ADVANCED_FACE ( 'NONE', ( #5134 ), #14726, .F. ) ;
#7577 = ORIENTED_EDGE ( 'NONE', *, *, #9978, .F. ) ;
#7578 = DIRECTION ( 'NONE',  ( 0.000000000000000000, 0.000000000000000000, 1.000000000000000000 ) ) ;
#7579 = VECTOR ( 'NONE', #5402, 1000.000000000000000 ) ;
#7580 = AXIS2_PLACEMENT_3D ( 'NONE', #13198, #2085, #8310 ) ;
#7581 = ORIENTED_EDGE ( 'NONE', *, *, #7651, .F. ) ;
#7582 = FACE_BOUND ( 'NONE', #8768, .T. ) ;
#7583 = EDGE_LOOP ( 'NONE', ( #17913, #10366, #16331, #15853, #6502 ) ) ;
#7584 = DIRECTION ( 'NONE',  ( -0.000000000000000000, -0.000000000000000000, 1.000000000000000000 ) ) ;
#7585 = DIRECTION ( 'NONE',  ( -1.000000000000000000, 0.000000000000000000, 7.065055611250995019E-15 ) ) ;
#7586 = DIRECTION ( 'NONE',  ( 0.000000000000000000, 0.000000000000000000, 1.000000000000000000 ) ) ;
#7587 = ADVANCED_FACE ( 'NONE', ( #5232 ), #11557, .F. ) ;
#7588 = CARTESIAN_POINT ( 'NONE',  ( -85.53020504959707182, -140.9188050298390067, 49.99999999999999289 ) ) ;
#7589 = CARTESIAN_POINT ( 'NONE',  ( 0.000000000000000000, 0.000000000000000000, -9.999999999999994671 ) ) ;
#7590 = ORIENTED_EDGE ( 'NONE', *, *, #9760, .T. ) ;
#7591 = ADVANCED_FACE ( 'NONE', ( #615 ), #14629, .F. ) ;
#7592 = DIRECTION ( 'NONE',  ( -0.2225209339563195554, 0.9749279121818223981, 0.000000000000000000 ) ) ;
#7593 = CYLINDRICAL_SURFACE ( 'NONE', #833, 150.0000000000000284 ) ;
#7594 = CARTESIAN_POINT ( 'NONE',  ( 134.3546152455197955, -75.63949198389357775, 5.121906984077789993 ) ) ;
#7595 = AXIS2_PLACEMENT_3D ( 'NONE', #6575, #14537, #19056 ) ;
#7596 = AXIS2_PLACEMENT_3D ( 'NONE', #12985, #175, #73 ) ;
#7597 = CARTESIAN_POINT ( 'NONE',  ( -62.09913334491130854, -10.11498556985139352, 293.5832628385307999 ) ) ;
#7598 = DIRECTION ( 'NONE',  ( 0.000000000000000000, 0.000000000000000000, -1.000000000000000000 ) ) ;
#7599 = CARTESIAN_POINT ( 'NONE',  ( -133.0181789769753777, -69.32831038615765351, 41.48694412335748183 ) ) ;
#7600 = VERTEX_POINT ( 'NONE', #19247 ) ;
#7601 = CYLINDRICAL_SURFACE ( 'NONE', #409, 99.99999999999997158 ) ;
#7602 = CIRCLE ( 'NONE', #7287, 160.0000000000000284 ) ;
#7603 = EDGE_CURVE ( 'NONE', #2409, #6948, #8586, .T. ) ;
#7604 = VERTEX_POINT ( 'NONE', #12887 ) ;
#7605 = ORIENTED_EDGE ( 'NONE', *, *, #685, .T. ) ;
#7606 = PRESENTATION_LAYER_ASSIGNMENT (  '', '', ( #11848 ) ) ;
#7607 = ORIENTED_EDGE ( 'NONE', *, *, #19651, .T. ) ;
#7608 = FACE_OUTER_BOUND ( 'NONE', #5370, .T. ) ;
#7609 = ADVANCED_FACE ( 'NONE', ( #8285 ), #11650, .F. ) ;
#7610 = DIRECTION ( 'NONE',  ( 1.000000000000000000, 0.000000000000000000, -0.000000000000000000 ) ) ;
#7611 = ORIENTED_EDGE ( 'NONE', *, *, #10229, .F. ) ;
#7612 = ADVANCED_FACE ( 'NONE', ( #19340 ), #11358, .F. ) ;
#7613 = AXIS2_PLACEMENT_3D ( 'NONE', #5684, #16826, #15286 ) ;
#7614 = CARTESIAN_POINT ( 'NONE',  ( 71.18887634719571622, -147.8252249328912740, 49.99999999999999289 ) ) ;
#7615 = DIRECTION ( 'NONE',  ( 0.4999999999999950040, 0.8660254037844415942, 0.000000000000000000 ) ) ;
#7616 = ADVANCED_FACE ( 'NONE', ( #16373 ), #10127, .F. ) ;
#7617 = ORIENTED_EDGE ( 'NONE', *, *, #18627, .T. ) ;
#7618 = CARTESIAN_POINT ( 'NONE',  ( 73.25972925305627825, -27.53920554013664912, 248.9926560891072143 ) ) ;
#7619 = CARTESIAN_POINT ( 'NONE',  ( -57.55901709132179178, -11.54977938102067547, 112.0427633081291816 ) ) ;
#7620 = DIRECTION ( 'NONE',  ( -0.000000000000000000, -0.000000000000000000, -1.000000000000000000 ) ) ;
#7621 = CARTESIAN_POINT ( 'NONE',  ( 73.82206860051529418, 25.99419088092216867, 132.4711112102474146 ) ) ;
#7622 = DIRECTION ( 'NONE',  ( -0.000000000000000000, -0.000000000000000000, 1.000000000000000000 ) ) ;
#7623 = AXIS2_PLACEMENT_3D ( 'NONE', #16153, #14902, #7136 ) ;
#7624 = CARTESIAN_POINT ( 'NONE',  ( 124.9958490023956301, -82.94424249022426920, 40.96431696885655782 ) ) ;
#7625 = CARTESIAN_POINT ( 'NONE',  ( -29.99999999999887379, 285.0000000000000568, 4.999999999999158007 ) ) ;
#7626 = ORIENTED_EDGE ( 'NONE', *, *, #4247, .F. ) ;
#7627 = ORIENTED_EDGE ( 'NONE', *, *, #11853, .F. ) ;
#7628 = ADVANCED_FACE ( 'NONE', ( #7059 ), #9925, .T. ) ;
#7629 = LINE ( 'NONE', #10486, #2802 ) ;
#7630 = ORIENTED_EDGE ( 'NONE', *, *, #4736, .T. ) ;
#7631 = VECTOR ( 'NONE', #6790, 1000.000000000000000 ) ;
#7632 = EDGE_LOOP ( 'NONE', ( #1235, #1308, #2670, #4333, #12869 ) ) ;
#7633 = CARTESIAN_POINT ( 'NONE',  ( -97.49999999999997158, -200.0000000000000000, 30.00000000000000000 ) ) ;
#7634 = AXIS2_PLACEMENT_3D ( 'NONE', #15834, #4995, #17478 ) ;
#7635 = ORIENTED_EDGE ( 'NONE', *, *, #6132, .F. ) ;
#7636 = CARTESIAN_POINT ( 'NONE',  ( 135.1060089022256818, -65.16414933467422088, 10.00000000000000355 ) ) ;
#7637 = CARTESIAN_POINT ( 'NONE',  ( 18.28567271940513450, -57.92709869106715814, 293.5832628385307999 ) ) ;
#7638 =( LENGTH_UNIT ( ) NAMED_UNIT ( * ) SI_UNIT ( .MILLI., .METRE. ) );
#7639 = CARTESIAN_POINT ( 'NONE',  ( 61.98599999999999000, 0.000000000000000000, 0.000000000000000000 ) ) ;
#7640 = ORIENTED_EDGE ( 'NONE', *, *, #3991, .F. ) ;
#7641 = ADVANCED_FACE ( 'NONE', ( #518 ), #6763, .F. ) ;
#7642 = EDGE_CURVE ( 'NONE', #13254, #2847, #18176, .T. ) ;
#7643 = CARTESIAN_POINT ( 'NONE',  ( 0.000000000000000000, 0.000000000000000000, 283.5832628385307999 ) ) ;
#7644 = CARTESIAN_POINT ( 'NONE',  ( 0.000000000000000000, 0.000000000000000000, 283.5832628385307999 ) ) ;
#7645 = EDGE_LOOP ( 'NONE', ( #17326, #1692, #6274, #14295 ) ) ;
#7646 = CARTESIAN_POINT ( 'NONE',  ( 5.485913980968119219, -1.678175111358107374, 293.5832628385307999 ) ) ;
#7647 = CARTESIAN_POINT ( 'NONE',  ( -28.06584155524100765, 53.86996498385663301, 283.5832628385307999 ) ) ;
#7648 = CIRCLE ( 'NONE', #8311, 3.224098631618458999 ) ;
#7649 = CARTESIAN_POINT ( 'NONE',  ( -107.5000000000000000, -1.734524432274993541E-14, 30.00000000000000000 ) ) ;
#7650 = VECTOR ( 'NONE', #11594, 1000.000000000000000 ) ;
#7651 = EDGE_CURVE ( 'NONE', #10388, #2887, #10539, .T. ) ;
#7652 = CYLINDRICAL_SURFACE ( 'NONE', #10052, 3.224098631618460331 ) ;
#7653 = CARTESIAN_POINT ( 'NONE',  ( -131.4993367897275789, -89.99660315853896009, 39.95156676386486083 ) ) ;
#7654 = FACE_OUTER_BOUND ( 'NONE', #11396, .T. ) ;
#7655 = ORIENTED_EDGE ( 'NONE', *, *, #12660, .T. ) ;
#7656 = FACE_BOUND ( 'NONE', #18254, .T. ) ;
#7657 = LINE ( 'NONE', #1210, #10881 ) ;
#7658 = ADVANCED_FACE ( 'NONE', ( #18808 ), #14192, .T. ) ;
#7659 = VERTEX_POINT ( 'NONE', #6428 ) ;
#7660 = EDGE_LOOP ( 'NONE', ( #5533, #19398, #3368, #6475 ) ) ;
#7661 = EDGE_CURVE ( 'NONE', #19189, #1562, #2022, .T. ) ;
#7662 = CARTESIAN_POINT ( 'NONE',  ( -62.18629025319808790, 9.564549117045718418, 293.5832628385307999 ) ) ;
#7663 = VECTOR ( 'NONE', #18821, 1000.000000000000000 ) ;
#7664 = VERTEX_POINT ( 'NONE', #17169 ) ;
#7665 = CARTESIAN_POINT ( 'NONE',  ( -22.29928840491073316, -56.50138340076681231, 283.5832628385307999 ) ) ;
#7666 = FACE_OUTER_BOUND ( 'NONE', #10804, .T. ) ;
#7667 = ORIENTED_EDGE ( 'NONE', *, *, #13910, .T. ) ;
#7668 = ADVANCED_FACE ( 'NONE', ( #12648 ), #18908, .F. ) ;
#7669 = CARTESIAN_POINT ( 'NONE',  ( 82.03125000000001421, -125.5821405433014064, 9.999999999999991118 ) ) ;
#7670 = LINE ( 'NONE', #3379, #2178 ) ;
#7671 = ADVANCED_FACE ( 'NONE', ( #277 ), #11214, .F. ) ;
#7672 = CYLINDRICAL_SURFACE ( 'NONE', #11118, 99.99999999999997158 ) ;
#7673 = ORIENTED_EDGE ( 'NONE', *, *, #457, .T. ) ;
#7674 = DIRECTION ( 'NONE',  ( -0.7430374143461878633, 0.6692498792541777819, 0.000000000000000000 ) ) ;
#7675 = AXIS2_PLACEMENT_3D ( 'NONE', #14363, #13015, #17544 ) ;
#7676 = CARTESIAN_POINT ( 'NONE',  ( 118.3534152657848608, 114.7431683447366595, 49.99999999999999289 ) ) ;
#7677 = FACE_BOUND ( 'NONE', #5725, .T. ) ;
#7678 = CARTESIAN_POINT ( 'NONE',  ( 99.45845524092791834, -131.3126558323551478, 35.94668960775785393 ) ) ;
#7679 = VERTEX_POINT ( 'NONE', #9684 ) ;
#7680 = DIRECTION ( 'NONE',  ( -0.2080686897406943958, -0.9781142164131909622, 0.000000000000000000 ) ) ;
#7681 = CARTESIAN_POINT ( 'NONE',  ( -62.18629025319808790, 9.564549117045714866, 248.9926560891072143 ) ) ;
#7682 = ORIENTED_EDGE ( 'NONE', *, *, #18231, .F. ) ;
#7683 = EDGE_LOOP ( 'NONE', ( #3477, #17134, #6817, #13691 ) ) ;
#7684 = DIRECTION ( 'NONE',  ( 0.000000000000000000, 0.000000000000000000, 1.000000000000000000 ) ) ;
#7685 = ORIENTED_EDGE ( 'NONE', *, *, #13024, .F. ) ;
#7686 = CARTESIAN_POINT ( 'NONE',  ( -99.09522870387660021, -131.8160711339301656, 4.567269884085281006 ) ) ;
#7687 = FACE_BOUND ( 'NONE', #11682, .T. ) ;
#7688 = ORIENTED_EDGE ( 'NONE', *, *, #11972, .T. ) ;
#7689 = DIRECTION ( 'NONE',  ( -0.000000000000000000, -0.000000000000000000, -1.000000000000000000 ) ) ;
#7690 = DIRECTION ( 'NONE',  ( 0.000000000000000000, 0.000000000000000000, -1.000000000000000000 ) ) ;
#7691 = CARTESIAN_POINT ( 'NONE',  ( -86.28560748592356333, -122.6989046848843969, 42.70417760891430703 ) ) ;
#7692 = CARTESIAN_POINT ( 'NONE',  ( 62.90240729679780429, 1.379293853802413983, 248.9926560891072143 ) ) ;
#7693 = CARTESIAN_POINT ( 'NONE',  ( -72.91900756452172061, 131.0832496385607158, -10.00000000000000178 ) ) ;
#7694 = CIRCLE ( 'NONE', #1150, 150.0000000000000284 ) ;
#7695 = ADVANCED_FACE ( 'NONE', ( #14086 ), #3252, .F. ) ;
#7696 = DIRECTION ( 'NONE',  ( 0.000000000000000000, 0.000000000000000000, -1.000000000000000000 ) ) ;
#7697 = CARTESIAN_POINT ( 'NONE',  ( -133.2712073793125001, -68.96827650305596080, 10.00000000000000888 ) ) ;
#7698 = CARTESIAN_POINT ( 'NONE',  ( 126.6625757374826549, -80.35588318643314665, -9.093145544296387328 ) ) ;
#7699 = DIRECTION ( 'NONE',  ( 0.000000000000000000, 0.000000000000000000, -1.000000000000000000 ) ) ;
#7700 = CIRCLE ( 'NONE', #20113, 62.91752772691707207 ) ;
#7701 = DIRECTION ( 'NONE',  ( -0.000000000000000000, -0.000000000000000000, 1.000000000000000000 ) ) ;
#7702 = CARTESIAN_POINT ( 'NONE',  ( -133.5474595738625680, -68.30173510457200337, 40.05649235983763390 ) ) ;
#7703 = EDGE_LOOP ( 'NONE', ( #9682, #497 ) ) ;
#7704 = CARTESIAN_POINT ( 'NONE',  ( 0.000000000000000000, 0.000000000000000000, 112.9440587442963562 ) ) ;
#7705 = EDGE_CURVE ( 'NONE', #7117, #4629, #12829, .T. ) ;
#7706 = ORIENTED_EDGE ( 'NONE', *, *, #13108, .F. ) ;
#7707 = VECTOR ( 'NONE', #5563, 1000.000000000000000 ) ;
#7708 = VERTEX_POINT ( 'NONE', #19107 ) ;
#7709 = VECTOR ( 'NONE', #11111, 1000.000000000000000 ) ;
#7710 = ORIENTED_EDGE ( 'NONE', *, *, #6618, .F. ) ;
#7711 = CIRCLE ( 'NONE', #7072, 7.500000000000007105 ) ;
#7712 = DIRECTION ( 'NONE',  ( 0.000000000000000000, 0.000000000000000000, -1.000000000000000000 ) ) ;
#7713 = LINE ( 'NONE', #3126, #3216 ) ;
#7714 = VERTEX_POINT ( 'NONE', #5096 ) ;
#7715 = CYLINDRICAL_SURFACE ( 'NONE', #11943, 27.50000000000000355 ) ;
#7716 = DIRECTION ( 'NONE',  ( -0.000000000000000000, -0.000000000000000000, 1.000000000000000000 ) ) ;
#7717 = EDGE_CURVE ( 'NONE', #9804, #14807, #479, .T. ) ;
#7718 = ORIENTED_EDGE ( 'NONE', *, *, #6258, .T. ) ;
#7719 = DIRECTION ( 'NONE',  ( 0.000000000000000000, -1.000000000000000000, 0.000000000000000000 ) ) ;
#7720 = EDGE_CURVE ( 'NONE', #7514, #7708, #20032, .T. ) ;
#7721 = DIRECTION ( 'NONE',  ( 0.000000000000000000, 0.000000000000000000, -1.000000000000000000 ) ) ;
#7722 = LINE ( 'NONE', #4880, #14013 ) ;
#7723 = CARTESIAN_POINT ( 'NONE',  ( -159.9599531637108782, -36.50981547337168109, 60.00000000000000000 ) ) ;
#7724 = DIRECTION ( 'NONE',  ( -0.3088643371590125697, 0.9511061040868803440, 0.000000000000000000 ) ) ;
#7725 = VECTOR ( 'NONE', #877, 1000.000000000000000 ) ;
#7726 = AXIS2_PLACEMENT_3D ( 'NONE', #8503, #16486, #16582 ) ;
#7727 = CARTESIAN_POINT ( 'NONE',  ( 133.9967726966432338, -77.99266392030685324, 36.52075283398300343 ) ) ;
#7728 = LINE ( 'NONE', #13969, #18501 ) ;
#7729 = EDGE_LOOP ( 'NONE', ( #1133, #706, #3491, #7560 ) ) ;
#7731 = ORIENTED_EDGE ( 'NONE', *, *, #11017, .T. ) ;
#7730 = VECTOR ( 'NONE', #2354, 1000.000000000000000 ) ;
#7732 = ADVANCED_FACE ( 'NONE', ( #2121 ), #14691, .F. ) ;
#7733 = VERTEX_POINT ( 'NONE', #3652 ) ;
#7734 = EDGE_CURVE ( 'NONE', #9156, #16671, #11614, .T. ) ;
#7735 = VERTEX_POINT ( 'NONE', #13234 ) ;
#7736 = EDGE_CURVE ( 'NONE', #9812, #6115, #773, .T. ) ;
#7737 = CARTESIAN_POINT ( 'NONE',  ( 167.4599531637113330, -36.50981547336952104, 49.99999999999999289 ) ) ;
#7738 = ORIENTED_EDGE ( 'NONE', *, *, #12166, .F. ) ;
#7739 = FACE_OUTER_BOUND ( 'NONE', #1397, .T. ) ;
#7740 = CARTESIAN_POINT ( 'NONE',  ( 67.36461649554532016, -39.84224160888924615, 248.9926560891072143 ) ) ;
#7741 = LINE ( 'NONE', #20120, #8621 ) ;
#7742 = LINE ( 'NONE', #16853, #12655 ) ;
#7743 = VERTEX_POINT ( 'NONE', #14882 ) ;
#7744 = CARTESIAN_POINT ( 'NONE',  ( 11.54085525628718401, 113.2974248684783163, 14.88498244535537296 ) ) ;
#7745 = DIRECTION ( 'NONE',  ( 1.000000000000000000, 0.000000000000000000, 0.000000000000000000 ) ) ;
#7746 = EDGE_CURVE ( 'NONE', #5045, #5530, #753, .T. ) ;
#7747 = ORIENTED_EDGE ( 'NONE', *, *, #20219, .F. ) ;
#7748 = AXIS2_PLACEMENT_3D ( 'NONE', #20240, #8166, #3166 ) ;
#7749 = EDGE_CURVE ( 'NONE', #7454, #13999, #2221, .T. ) ;
#7750 = DIRECTION ( 'NONE',  ( -0.4999999999999888423, -0.8660254037844449249, -0.000000000000000000 ) ) ;
#7751 = LINE ( 'NONE', #17384, #19241 ) ;
#7752 = DIRECTION ( 'NONE',  ( -0.000000000000000000, -0.000000000000000000, 1.000000000000000000 ) ) ;
#7753 = CARTESIAN_POINT ( 'NONE',  ( 0.000000000000000000, 0.000000000000000000, -10.00000000000000178 ) ) ;
#7754 = DIRECTION ( 'NONE',  ( -0.000000000000000000, -0.000000000000000000, 1.000000000000000000 ) ) ;
#7755 = CARTESIAN_POINT ( 'NONE',  ( 159.9599531637113330, -36.50981547336952104, 39.99999999999999289 ) ) ;
#7756 = ORIENTED_EDGE ( 'NONE', *, *, #1535, .F. ) ;
#7757 = FACE_BOUND ( 'NONE', #12267, .T. ) ;
#7758 = VERTEX_POINT ( 'NONE', #9016 ) ;
#7759 =( REPRESENTATION_RELATIONSHIP ('NONE','NONE', #17382, #15821 ) REPRESENTATION_RELATIONSHIP_WITH_TRANSFORMATION ( #8296 )SHAPE_REPRESENTATION_RELATIONSHIP( ) );
#7760 = ADVANCED_FACE ( 'NONE', ( #2418 ), #7486, .F. ) ;
#7761 = AXIS2_PLACEMENT_3D ( 'NONE', #15632, #11116, #2023 ) ;
#7762 = EDGE_CURVE ( 'NONE', #2440, #17104, #1060, .T. ) ;
#7763 = ORIENTED_EDGE ( 'NONE', *, *, #15652, .F. ) ;
#7764 = EDGE_CURVE ( 'NONE', #19299, #14265, #9986, .T. ) ;
#7765 = DIRECTION ( 'NONE',  ( 1.000000000000000000, 0.000000000000000000, 0.000000000000000000 ) ) ;
#7766 = VERTEX_POINT ( 'NONE', #8647 ) ;
#7767 = CARTESIAN_POINT ( 'NONE',  ( -111.9753657172487635, 86.11583021959165762, -34.99999999999998579 ) ) ;
#7768 = DIRECTION ( 'NONE',  ( -0.000000000000000000, -0.000000000000000000, -1.000000000000000000 ) ) ;
#7769 = VERTEX_POINT ( 'NONE', #5292 ) ;
#7770 = DIRECTION ( 'NONE',  ( 1.000000000000000000, 0.000000000000000000, 0.000000000000000000 ) ) ;
#7771 = DIRECTION ( 'NONE',  ( 1.000000000000000000, 0.000000000000000000, 0.000000000000000000 ) ) ;
#7772 = EDGE_CURVE ( 'NONE', #9468, #11620, #18063, .T. ) ;
#7773 = AXIS2_PLACEMENT_3D ( 'NONE', #8550, #14789, #14593 ) ;
#7774 = DIRECTION ( 'NONE',  ( -0.000000000000000000, -1.000000000000000000, -0.000000000000000000 ) ) ;
#7775 = CARTESIAN_POINT ( 'NONE',  ( -68.46530598706767989, 37.93579148621533648, 248.9926560891072143 ) ) ;
#7776 = VECTOR ( 'NONE', #16767, 1000.000000000000000 ) ;
#7777 = ORIENTED_EDGE ( 'NONE', *, *, #1420, .F. ) ;
#7778 = CARTESIAN_POINT ( 'NONE',  ( 112.4320812185962524, -22.51277856475483574, 14.88498244535466775 ) ) ;
#7779 = DIRECTION ( 'NONE',  ( 0.000000000000000000, 1.000000000000000000, 0.000000000000000000 ) ) ;
#7780 = DIRECTION ( 'NONE',  ( 0.9749279121818227312, 0.2225209339563182231, -0.000000000000000000 ) ) ;
#7781 = CARTESIAN_POINT ( 'NONE',  ( 96.67218534449422407, -115.8154871359606375, 29.72277444615395936 ) ) ;
#7782 = ORIENTED_EDGE ( 'NONE', *, *, #3853, .T. ) ;
#7783 = DIRECTION ( 'NONE',  ( 1.000000000000000000, 0.000000000000000000, 0.000000000000000000 ) ) ;
#7784 = CARTESIAN_POINT ( 'NONE',  ( 130.9868171408399462, -91.88282611735539263, 0.000000000000000000 ) ) ;
#7785 = EDGE_CURVE ( 'NONE', #1681, #1353, #3699, .T. ) ;
#7786 = ADVANCED_FACE ( 'NONE', ( #3743 ), #12078, .T. ) ;
#7787 = ORIENTED_EDGE ( 'NONE', *, *, #14261, .T. ) ;
#7788 = ORIENTED_EDGE ( 'NONE', *, *, #9797, .F. ) ;
#7789 = ORIENTED_EDGE ( 'NONE', *, *, #19162, .F. ) ;
#7790 = DIRECTION ( 'NONE',  ( 0.000000000000000000, 0.000000000000000000, 1.000000000000000000 ) ) ;
#7791 = AXIS2_PLACEMENT_3D ( 'NONE', #10495, #11823, #16748 ) ;
#7792 = AXIS2_PLACEMENT_3D ( 'NONE', #2492, #10256, #7199 ) ;
#7793 = EDGE_LOOP ( 'NONE', ( #13389, #19862, #529, #19927 ) ) ;
#7794 = AXIS2_PLACEMENT_3D ( 'NONE', #2957, #19623, #3163 ) ;
#7795 = ADVANCED_FACE ( 'NONE', ( #5864 ), #3939, .T. ) ;
#7796 = DIRECTION ( 'NONE',  ( 1.000000000000000000, 0.000000000000000000, 0.000000000000000000 ) ) ;
#7797 = VECTOR ( 'NONE', #9864, 1000.000000000000000 ) ;
#7798 = FACE_BOUND ( 'NONE', #8602, .T. ) ;
#7799 = ORIENTED_EDGE ( 'NONE', *, *, #8477, .T. ) ;
#7800 = DIRECTION ( 'NONE',  ( 0.4999999999999979461, 0.8660254037844398178, 0.000000000000000000 ) ) ;
#7801 = CYLINDRICAL_SURFACE ( 'NONE', #14834, 60.74260934110282051 ) ;
#7802 = CYLINDRICAL_SURFACE ( 'NONE', #5707, 6.000000000000001776 ) ;
#7803 = CARTESIAN_POINT ( 'NONE',  ( -96.05830942202625522, -116.0381168402466159, 30.26647072828682639 ) ) ;
#7804 = CARTESIAN_POINT ( 'NONE',  ( 81.66698895276879000, 79.37254397626031732, 14.88498244535488269 ) ) ;
#7805 = CARTESIAN_POINT ( 'NONE',  ( 87.10655032386927132, -147.8252249328912740, 39.99999999999999289 ) ) ;
#7806 = FACE_OUTER_BOUND ( 'NONE', #5385, .T. ) ;
#7807 = FACE_OUTER_BOUND ( 'NONE', #9677, .T. ) ;
#7808 = CARTESIAN_POINT ( 'NONE',  ( 0.000000000000000000, 0.000000000000000000, 293.5832628385307999 ) ) ;
#7809 = DIRECTION ( 'NONE',  ( 6.982962677686266711E-15, -0.000000000000000000, 1.000000000000000000 ) ) ;
#7810 = CARTESIAN_POINT ( 'NONE',  ( -109.9999999999983515, 275.0000000000000000, 85.00000000000001421 ) ) ;
#7811 = CARTESIAN_POINT ( 'NONE',  ( -132.9666886943602719, -83.66363014847074453, 38.85988273695094364 ) ) ;
#7812 = CIRCLE ( 'NONE', #9765, 7.500000000000020428 ) ;
#7813 = EDGE_LOOP ( 'NONE', ( #2841, #19348, #8677 ) ) ;
#7814 = CARTESIAN_POINT ( 'NONE',  ( 42.50000000000000000, 0.000000000000000000, -100.0000000000000000 ) ) ;
#7815 = ORIENTED_EDGE ( 'NONE', *, *, #14835, .T. ) ;
#7816 = ORIENTED_EDGE ( 'NONE', *, *, #14480, .T. ) ;
#7817 = ORIENTED_EDGE ( 'NONE', *, *, #5035, .F. ) ;
#7818 = VECTOR ( 'NONE', #5736, 1000.000000000000227 ) ;
#7819 = AXIS2_PLACEMENT_3D ( 'NONE', #8826, #4223, #11689 ) ;
#7820 = DIRECTION ( 'NONE',  ( 0.9396926207859082059, 0.3420201433256694901, 0.000000000000000000 ) ) ;
#7821 = CARTESIAN_POINT ( 'NONE',  ( 0.000000000000000000, 0.000000000000000000, -115.0000000000000000 ) ) ;
#7822 = LINE ( 'NONE', #4559, #13045 ) ;
#7823 = ORIENTED_EDGE ( 'NONE', *, *, #9670, .T. ) ;
#7824 = CARTESIAN_POINT ( 'NONE',  ( -109.9999999999874376, 73.61623156955475622, -29.99999999999998579 ) ) ;
#7825 = CARTESIAN_POINT ( 'NONE',  ( 19.23614321207236699, -57.61627707419557964, 293.5832628385307999 ) ) ;
#7826 = DIRECTION ( 'NONE',  ( 0.000000000000000000, 0.000000000000000000, 1.000000000000000000 ) ) ;
#7827 = CARTESIAN_POINT ( 'NONE',  ( -67.08601213326565471, -40.32479851956794192, 132.4711112102474146 ) ) ;
#7828 = DIRECTION ( 'NONE',  ( -0.7660444431189792347, 0.6427876096865379196, 0.000000000000000000 ) ) ;
#7829 = VERTEX_POINT ( 'NONE', #5386 ) ;
#7830 = CARTESIAN_POINT ( 'NONE',  ( 132.3052566686612863, -70.67971788940297984, 43.04150566780438680 ) ) ;
#7831 = LINE ( 'NONE', #14076, #19805 ) ;
#7832 = EDGE_LOOP ( 'NONE', ( #9581, #12896, #16262 ) ) ;
#7833 = ORIENTED_EDGE ( 'NONE', *, *, #15079, .F. ) ;
#7834 = EDGE_LOOP ( 'NONE', ( #1698, #14973, #16189, #17820, #4651 ) ) ;
#7835 = VERTEX_POINT ( 'NONE', #18340 ) ;
#7836 = EDGE_CURVE ( 'NONE', #16766, #7758, #4314, .T. ) ;
#7837 = PRODUCT_DEFINITION_SHAPE ( 'NONE', 'NONE',  #3275 ) ;
#7838 = ORIENTED_EDGE ( 'NONE', *, *, #10639, .T. ) ;
#7839 = FACE_OUTER_BOUND ( 'NONE', #10566, .T. ) ;
#7840 = CARTESIAN_POINT ( 'NONE',  ( -100.4560359297607874, -129.9019447003570349, 37.10626013476207419 ) ) ;
#7841 = CARTESIAN_POINT ( 'NONE',  ( 0.000000000000000000, 0.000000000000000000, 283.5832628385307999 ) ) ;
#7842 = CIRCLE ( 'NONE', #2312, 7.500000000000006217 ) ;
#7843 = LINE ( 'NONE', #4900, #13176 ) ;
#7844 = FACE_OUTER_BOUND ( 'NONE', #14129, .T. ) ;
#7845 = ORIENTED_EDGE ( 'NONE', *, *, #10494, .T. ) ;
#7846 = VECTOR ( 'NONE', #12059, 1000.000000000000114 ) ;
#7847 = DIRECTION ( 'NONE',  ( 0.000000000000000000, 0.000000000000000000, -1.000000000000000000 ) ) ;
#7848 = LINE ( 'NONE', #11619, #5536 ) ;
#7849 = ORIENTED_EDGE ( 'NONE', *, *, #2349, .T. ) ;
#7850 = EDGE_CURVE ( 'NONE', #9758, #5816, #16804, .T. ) ;
#7851 = UNCERTAINTY_MEASURE_WITH_UNIT (LENGTH_MEASURE( 1.000000000000000082E-05 ), #10342, 'distance_accuracy_value', 'NONE');
#7852 = CARTESIAN_POINT ( 'NONE',  ( 126.5370453525553671, 80.55045718954892209, 49.99999999999999289 ) ) ;
#7853 = DIRECTION ( 'NONE',  ( 0.000000000000000000, 0.000000000000000000, 1.000000000000000000 ) ) ;
#7854 = EDGE_CURVE ( 'NONE', #6551, #12474, #16333, .T. ) ;
#7855 = ADVANCED_FACE ( 'NONE', ( #1250 ), #1670, .F. ) ;
#7856 = CARTESIAN_POINT ( 'NONE',  ( 0.000000000000000000, 0.000000000000000000, 293.5832628385307999 ) ) ;
#7857 = DIRECTION ( 'NONE',  ( 1.000000000000000000, 0.000000000000000000, 0.000000000000000000 ) ) ;
#7858 = DIRECTION ( 'NONE',  ( -0.000000000000000000, -0.000000000000000000, -1.000000000000000000 ) ) ;
#7859 = DIRECTION ( 'NONE',  ( 0.000000000000000000, 0.000000000000000000, 1.000000000000000000 ) ) ;
#7860 = VERTEX_POINT ( 'NONE', #16905 ) ;
#7861 = DIRECTION ( 'NONE',  ( -0.000000000000000000, -0.000000000000000000, 1.000000000000000000 ) ) ;
#7862 = ORIENTED_EDGE ( 'NONE', *, *, #18627, .F. ) ;
#7863 = AXIS2_PLACEMENT_3D ( 'NONE', #19243, #5519, #16370 ) ;
#7864 = VERTEX_POINT ( 'NONE', #8000 ) ;
#7865 = ADVANCED_FACE ( 'NONE', ( #2896 ), #13931, .T. ) ;
#7866 = DIRECTION ( 'NONE',  ( 0.000000000000000000, 0.000000000000000000, -1.000000000000000000 ) ) ;
#7867 = ORIENTED_EDGE ( 'NONE', *, *, #19137, .F. ) ;
#7868 = CARTESIAN_POINT ( 'NONE',  ( -120.9637972807140045, 75.12262024236758862, -33.48191611480011431 ) ) ;
#7869 = FACE_OUTER_BOUND ( 'NONE', #11820, .T. ) ;
#7870 = ORIENTED_EDGE ( 'NONE', *, *, #14431, .F. ) ;
#7871 = CARTESIAN_POINT ( 'NONE',  ( 82.07017599500315441, -125.5567397147592743, 8.511632757311264896 ) ) ;
#7872 = CARTESIAN_POINT ( 'NONE',  ( -39.84224160888947353, -67.36461649554519227, 248.9926560891072143 ) ) ;
#7873 = VECTOR ( 'NONE', #17689, 999.9999999999998863 ) ;
#7874 = ADVANCED_FACE ( 'NONE', ( #12597 ), #1563, .F. ) ;
#7875 = EDGE_CURVE ( 'NONE', #19407, #7835, #20176, .T. ) ;
#7876 = EDGE_CURVE ( 'NONE', #17725, #4372, #16434, .T. ) ;
#7877 = CARTESIAN_POINT ( 'NONE',  ( 44.07268132743672595, 38.78191089773085309, 110.7293897666001214 ) ) ;
#7878 = CARTESIAN_POINT ( 'NONE',  ( 0.000000000000000000, 0.000000000000000000, 49.99999999999999289 ) ) ;
#7879 = EDGE_LOOP ( 'NONE', ( #8665, #19810, #5330, #3624 ) ) ;
#7880 = CARTESIAN_POINT ( 'NONE',  ( -110.0000000000000142, 275.0000000000000000, -29.99999999999998224 ) ) ;
#7881 = CARTESIAN_POINT ( 'NONE',  ( -51.36153797460868731, 59.06449708980215973, 132.4711112102474146 ) ) ;
#7882 = FACE_OUTER_BOUND ( 'NONE', #11342, .T. ) ;
#7883 = CARTESIAN_POINT ( 'NONE',  ( 98.30983243222797796, -132.8827373471760893, 33.95839073212757597 ) ) ;
#7884 = ORIENTED_EDGE ( 'NONE', *, *, #9396, .T. ) ;
#7885 = CARTESIAN_POINT ( 'NONE',  ( -110.0000000000000142, 265.0000000000000000, -75.00000000000000000 ) ) ;
#7886 = CARTESIAN_POINT ( 'NONE',  ( -70.08028827194087285, 132.6226048388235199, 2.306676233856181479 ) ) ;
#7887 = ORIENTED_EDGE ( 'NONE', *, *, #1123, .F. ) ;
#7888 = ORIENTED_EDGE ( 'NONE', *, *, #2753, .T. ) ;
#7889 = VERTEX_POINT ( 'NONE', #1460 ) ;
#7890 = EDGE_CURVE ( 'NONE', #20169, #19329, #12495, .T. ) ;
#7891 = CARTESIAN_POINT ( 'NONE',  ( -190.0000000000000000, 292.9500000000000455, 5.000000000000309974 ) ) ;
#7892 = ORIENTED_EDGE ( 'NONE', *, *, #12134, .F. ) ;
#7893 = CARTESIAN_POINT ( 'NONE',  ( -97.67667160654316660, -133.7228621772585484, 8.114239421803903340 ) ) ;
#7894 = FACE_BOUND ( 'NONE', #7285, .T. ) ;
#7895 = ORIENTED_EDGE ( 'NONE', *, *, #13573, .F. ) ;
#7896 = CARTESIAN_POINT ( 'NONE',  ( 128.2779226595531270, 102.2982297021113141, 49.99999999999999289 ) ) ;
#7897 = CARTESIAN_POINT ( 'NONE',  ( -110.0000000000000142, 265.0000000000000000, 5.000000000000000888 ) ) ;
#7898 = DIRECTION ( 'NONE',  ( 1.000000000000000000, 0.000000000000000000, 0.000000000000000000 ) ) ;
#7899 = CARTESIAN_POINT ( 'NONE',  ( -89.41054993673267859, -120.4453604907586310, 45.95706278337525674 ) ) ;
#7900 = EDGE_CURVE ( 'NONE', #1487, #15959, #17331, .T. ) ;
#7901 = CARTESIAN_POINT ( 'NONE',  ( 77.21438937758502163, 12.78021302872874010, 132.4711112102474146 ) ) ;
#7902 = EDGE_CURVE ( 'NONE', #1787, #14365, #14470, .T. ) ;
#7903 = CARTESIAN_POINT ( 'NONE',  ( -98.63291732527035549, -113.0135401039851786, -9.876607713649601550 ) ) ;
#7904 = DIRECTION ( 'NONE',  ( 1.613511099790691498E-16, -1.000000000000000000, 0.000000000000000000 ) ) ;
#7905 = FACE_OUTER_BOUND ( 'NONE', #4305, .T. ) ;
#7906 = DIRECTION ( 'NONE',  ( -0.000000000000000000, -0.000000000000000000, 1.000000000000000000 ) ) ;
#7907 = CARTESIAN_POINT ( 'NONE',  ( -131.9259051260646629, -88.29481989230392003, 39.77911086439604560 ) ) ;
#7908 = EDGE_CURVE ( 'NONE', #4730, #4430, #6071, .T. ) ;
#7909 = ORIENTED_EDGE ( 'NONE', *, *, #11561, .F. ) ;
#7910 = DIRECTION ( 'NONE',  ( 0.000000000000000000, 0.000000000000000000, 1.000000000000000000 ) ) ;
#7911 = VECTOR ( 'NONE', #3535, 1000.000000000000000 ) ;
#7912 = EDGE_CURVE ( 'NONE', #10504, #17700, #6320, .T. ) ;
#7913 = VERTEX_POINT ( 'NONE', #20071 ) ;
#7914 = ORIENTED_EDGE ( 'NONE', *, *, #3980, .T. ) ;
#7915 = ORIENTED_EDGE ( 'NONE', *, *, #1389, .T. ) ;
#7916 = CARTESIAN_POINT ( 'NONE',  ( -55.16472960512350454, 30.25670013172272377, 293.5832628385307999 ) ) ;
#7917 = FACE_OUTER_BOUND ( 'NONE', #3836, .T. ) ;
#7918 = AXIS2_PLACEMENT_3D ( 'NONE', #8186, #14334, #14434 ) ;
#7919 = CARTESIAN_POINT ( 'NONE',  ( -47.22802745636877120, -134.7565053399285091, 39.99999999999999289 ) ) ;
#7920 = CARTESIAN_POINT ( 'NONE',  ( 15.91767397667354089, 149.1530343478547422, 60.00000000000000000 ) ) ;
#7921 = EDGE_LOOP ( 'NONE', ( #16328, #14035, #14267, #13897 ) ) ;
#7922 = CARTESIAN_POINT ( 'NONE',  ( -17.24542129382122724, 20.55229278271246329, 14.88498244535557369 ) ) ;
#7923 = CARTESIAN_POINT ( 'NONE',  ( 17.49999999999999289, 0.000000000000000000, 39.88498244535532677 ) ) ;
#7924 = LINE ( 'NONE', #4453, #20216 ) ;
#7925 = CIRCLE ( 'NONE', #13459, 62.91752772691707207 ) ;
#7926 = DIRECTION ( 'NONE',  ( 0.1736481776669273613, 0.9848077530122086864, 0.000000000000000000 ) ) ;
#7927 = DIRECTION ( 'NONE',  ( 1.000000000000000000, 0.000000000000000000, 0.000000000000000000 ) ) ;
#7928 = EDGE_CURVE ( 'NONE', #16974, #4062, #13826, .T. ) ;
#7929 = ORIENTED_EDGE ( 'NONE', *, *, #14238, .F. ) ;
#7930 = CARTESIAN_POINT ( 'NONE',  ( 134.6114153021046320, -66.18050771012664768, 35.86948590222475985 ) ) ;
#7931 = CARTESIAN_POINT ( 'NONE',  ( 133.3649390995069268, -81.63041515106810664, 38.20349535801842933 ) ) ;
#7932 = ORIENTED_EDGE ( 'NONE', *, *, #9841, .F. ) ;
#7933 = ORIENTED_EDGE ( 'NONE', *, *, #2845, .F. ) ;
#7934 = VECTOR ( 'NONE', #1347, 1000.000000000000000 ) ;
#7935 = AXIS2_PLACEMENT_3D ( 'NONE', #10652, #3309, #17222 ) ;
#7936 = ORIENTED_EDGE ( 'NONE', *, *, #17235, .F. ) ;
#7937 = ORIENTED_EDGE ( 'NONE', *, *, #18680, .T. ) ;
#7938 = CARTESIAN_POINT ( 'NONE',  ( 57.61823435390807902, 19.23677882349220880, 283.5832628385307999 ) ) ;
#7939 = VERTEX_POINT ( 'NONE', #18544 ) ;
#7940 = CARTESIAN_POINT ( 'NONE',  ( 0.000000000000000000, 0.000000000000000000, 283.5832628385307999 ) ) ;
#7941 = VECTOR ( 'NONE', #194, 1000.000000000000000 ) ;
#7942 = CARTESIAN_POINT ( 'NONE',  ( -97.67856431661350314, -133.7203759155860894, 31.89566238906889240 ) ) ;
#7943 = FACE_BOUND ( 'NONE', #3642, .T. ) ;
#7944 =( NAMED_UNIT ( * ) SI_UNIT ( $, .STERADIAN. ) SOLID_ANGLE_UNIT ( ) );
#7945 = AXIS2_PLACEMENT_3D ( 'NONE', #12676, #9411, #14111 ) ;
#7946 = FACE_OUTER_BOUND ( 'NONE', #6374, .T. ) ;
#7947 = ORIENTED_EDGE ( 'NONE', *, *, #16413, .T. ) ;
#7948 = LINE ( 'NONE', #12551, #19746 ) ;
#7949 = CARTESIAN_POINT ( 'NONE',  ( 0.8038475772933632024, 5.196152422706628471, 9.000000000000001776 ) ) ;
#7950 = ORIENTED_EDGE ( 'NONE', *, *, #7147, .T. ) ;
#7951 = DIRECTION ( 'NONE',  ( -0.000000000000000000, -0.000000000000000000, 1.000000000000000000 ) ) ;
#7953 = AXIS2_PLACEMENT_3D ( 'NONE', #10417, #15128, #8984 ) ;
#7952 = DIRECTION ( 'NONE',  ( 1.000000000000000000, 0.000000000000000000, 0.000000000000000000 ) ) ;
#7954 = CARTESIAN_POINT ( 'NONE',  ( 19.30071112029679625, -55.43188410062176530, 132.4711112102474146 ) ) ;
#7955 = ADVANCED_FACE ( 'NONE', ( #12290 ), #18759, .F. ) ;
#7956 = DIRECTION ( 'NONE',  ( 0.8660254037844398178, -0.4999999999999979461, 0.000000000000000000 ) ) ;
#7957 = DIRECTION ( 'NONE',  ( 6.982962677686266711E-15, -0.000000000000000000, 1.000000000000000000 ) ) ;
#7958 = AXIS2_PLACEMENT_3D ( 'NONE', #5384, #6623, #17866 ) ;
#7959 = FACE_OUTER_BOUND ( 'NONE', #10064, .T. ) ;
#7960 = CARTESIAN_POINT ( 'NONE',  ( -77.07195518394449607, 116.8771345694330108, -6.980692854872754260 ) ) ;
#7961 = EDGE_LOOP ( 'NONE', ( #19130, #19931, #15839, #9361 ) ) ;
#7962 = LINE ( 'NONE', #17594, #14800 ) ;
#7963 = VECTOR ( 'NONE', #17502, 1000.000000000000000 ) ;
#7964 = ORIENTED_EDGE ( 'NONE', *, *, #145, .T. ) ;
#7965 = VERTEX_POINT ( 'NONE', #4528 ) ;
#7966 = DIRECTION ( 'NONE',  ( -0.5000000000000069944, 0.8660254037844345998, 0.000000000000000000 ) ) ;
#7967 = ADVANCED_FACE ( 'NONE', ( #129 ), #3000, .F. ) ;
#7968 = ORIENTED_EDGE ( 'NONE', *, *, #3401, .F. ) ;
#7969 = CARTESIAN_POINT ( 'NONE',  ( -125.8454112683333506, 69.15288340776045573, -31.78671230953092319 ) ) ;
#7970 = DIRECTION ( 'NONE',  ( 0.000000000000000000, 0.000000000000000000, 1.000000000000000000 ) ) ;
#7971 = VERTEX_POINT ( 'NONE', #17115 ) ;
#7972 = CIRCLE ( 'NONE', #17471, 7.500000000000007105 ) ;
#7973 =( LENGTH_UNIT ( ) NAMED_UNIT ( * ) SI_UNIT ( .MILLI., .METRE. ) );
#7974 = CARTESIAN_POINT ( 'NONE',  ( -14.39940464655760799, -76.92888220842480962, 132.4711112102474146 ) ) ;
#7975 = CARTESIAN_POINT ( 'NONE',  ( -32.64570716507502368, 53.78543575132162857, 248.9926560891072143 ) ) ;
#7976 = VECTOR ( 'NONE', #10089, 999.9999999999998863 ) ;
#7977 = EDGE_CURVE ( 'NONE', #6462, #1353, #3101, .T. ) ;
#7978 = CARTESIAN_POINT ( 'NONE',  ( -170.2125097089225960, -199.3942630591407692, 0.000000000000000000 ) ) ;
#7979 = CARTESIAN_POINT ( 'NONE',  ( 73.82206860051529418, 25.99419088092216867, 111.4180192758973362 ) ) ;
#7980 = ORIENTED_EDGE ( 'NONE', *, *, #6662, .F. ) ;
#7981 = DIRECTION ( 'NONE',  ( -0.8660254037844397068, 0.4999999999999978906, 0.000000000000000000 ) ) ;
#7982 = CARTESIAN_POINT ( 'NONE',  ( -166.7850001792984926, -200.0000000000000284, 0.000000000000000000 ) ) ;
#7983 = DIRECTION ( 'NONE',  ( 0.000000000000000000, 0.000000000000000000, 1.000000000000000000 ) ) ;
#7984 = DIRECTION ( 'NONE',  ( 0.000000000000000000, 1.000000000000000000, 0.000000000000000000 ) ) ;
#7985 = ORIENTED_EDGE ( 'NONE', *, *, #9851, .T. ) ;
#7986 = DIRECTION ( 'NONE',  ( 0.000000000000000000, 0.000000000000000000, -1.000000000000000000 ) ) ;
#7987 = CARTESIAN_POINT ( 'NONE',  ( -103.6230814261940623, 108.4577647952326487, 44.49395664845071252 ) ) ;
#7988 = ORIENTED_EDGE ( 'NONE', *, *, #2012, .F. ) ;
#7989 = VECTOR ( 'NONE', #16666, 1000.000000000000000 ) ;
#7990 = EDGE_LOOP ( 'NONE', ( #71, #10573, #18297, #13670 ) ) ;
#7991 = ORIENTED_EDGE ( 'NONE', *, *, #17156, .F. ) ;
#7992 = CARTESIAN_POINT ( 'NONE',  ( 0.000000000000000000, 0.000000000000000000, 0.000000000000000000 ) ) ;
#7993 = EDGE_CURVE ( 'NONE', #2635, #9958, #1766, .T. ) ;
#7994 = ORIENTED_EDGE ( 'NONE', *, *, #3840, .F. ) ;
#7995 = EDGE_CURVE ( 'NONE', #13722, #11567, #10962, .T. ) ;
#7996 = CARTESIAN_POINT ( 'NONE',  ( -104.3997176008718810, -123.8500140569469181, 0.4893052421375900241 ) ) ;
#7997 = CARTESIAN_POINT ( 'NONE',  ( -136.7839808106123485, 61.60861089918629574, 34.73673964685640669 ) ) ;
#7998 = ORIENTED_EDGE ( 'NONE', *, *, #9541, .T. ) ;
#7999 = VECTOR ( 'NONE', #1565, 1000.000000000000114 ) ;
#8000 = CARTESIAN_POINT ( 'NONE',  ( 106.5208805777952676, 53.25886146954521649, 14.88498244535470683 ) ) ;
#8001 = DIRECTION ( 'NONE',  ( 0.000000000000000000, 0.000000000000000000, 1.000000000000000000 ) ) ;
#8002 = DIRECTION ( 'NONE',  ( -0.000000000000000000, -0.000000000000000000, 1.000000000000000000 ) ) ;
#8003 = CARTESIAN_POINT ( 'NONE',  ( -96.25732604711518547, -115.9704170962522198, 30.03172575643280595 ) ) ;
#8004 = VECTOR ( 'NONE', #18500, 1000.000000000000000 ) ;
#8005 = LINE ( 'NONE', #14250, #3473 ) ;
#8006 = CARTESIAN_POINT ( 'NONE',  ( -90.67862352884070276, -119.4897427140443682, -6.860445880948178754 ) ) ;
#8007 = EDGE_CURVE ( 'NONE', #4788, #10, #11170, .T. ) ;
#8008 = CARTESIAN_POINT ( 'NONE',  ( -61.81362617575094021, 11.73417718768112294, 248.9926560891072143 ) ) ;
#8009 = CARTESIAN_POINT ( 'NONE',  ( -56.84754764479025368, -154.7316448359455308, 49.99999999999999289 ) ) ;
#8010 = CARTESIAN_POINT ( 'NONE',  ( 176.1792632384392334, -186.5724904703758682, 30.00000000000000000 ) ) ;
#8011 = CARTESIAN_POINT ( 'NONE',  ( -134.0015816819225165, -77.97298368087619735, 36.53274635918683799 ) ) ;
#8012 = ORIENTED_EDGE ( 'NONE', *, *, #19258, .F. ) ;
#8013 = CARTESIAN_POINT ( 'NONE',  ( -123.2780666175815298, 53.67120218771228934, -27.39856999340311106 ) ) ;
#8014 = VECTOR ( 'NONE', #4608, 1000.000000000000114 ) ;
#8015 = ORIENTED_EDGE ( 'NONE', *, *, #17243, .F. ) ;
#8016 = EDGE_CURVE ( 'NONE', #2113, #16938, #9255, .T. ) ;
#8017 = EDGE_CURVE ( 'NONE', #7913, #4516, #2278, .T. ) ;
#8018 = ORIENTED_EDGE ( 'NONE', *, *, #12852, .F. ) ;
#8019 = EDGE_CURVE ( 'NONE', #2515, #19514, #635, .T. ) ;
#8020 = ORIENTED_EDGE ( 'NONE', *, *, #7228, .F. ) ;
#8021 = CARTESIAN_POINT ( 'NONE',  ( -142.7819598182928189, -16.97992044938526490, 17.29344121494534647 ) ) ;
#8022 = AXIS2_PLACEMENT_3D ( 'NONE', #13940, #18450, #16917 ) ;
#8023 = CARTESIAN_POINT ( 'NONE',  ( 163.5019688434126977, -20.99123081650019884, 60.00000000000000000 ) ) ;
#8024 = DIRECTION ( 'NONE',  ( 0.000000000000000000, 0.000000000000000000, 1.000000000000000000 ) ) ;
#8025 = CARTESIAN_POINT ( 'NONE',  ( 60.22232964560483737, 7.948937137877944537, 283.5832628385307999 ) ) ;
#8026 = LINE ( 'NONE', #11403, #17967 ) ;
#8027 = DIRECTION ( 'NONE',  ( 0.000000000000000000, 0.000000000000000000, 1.000000000000000000 ) ) ;
#8028 = EDGE_CURVE ( 'NONE', #9259, #807, #18966, .T. ) ;
#8029 = CARTESIAN_POINT ( 'NONE',  ( -103.8888757476051836, -46.65403860089418941, 39.88498244535617943 ) ) ;
#8030 = DIRECTION ( 'NONE',  ( 0.000000000000000000, 0.000000000000000000, 1.000000000000000000 ) ) ;
#8031 = CARTESIAN_POINT ( 'NONE',  ( -81.99056186900656940, -84.64042930812179577, 39.88498244535603021 ) ) ;
#8032 = CARTESIAN_POINT ( 'NONE',  ( -2.629322876227788264, -60.68773558783006905, 283.5832628385307999 ) ) ;
#8033 = EDGE_LOOP ( 'NONE', ( #11884, #4691, #18337, #17189 ) ) ;
#8034 = FACE_OUTER_BOUND ( 'NONE', #11066, .T. ) ;
#8035 = DIRECTION ( 'NONE',  ( -1.000000000000000000, 0.000000000000000000, 0.000000000000000000 ) ) ;
#8036 = CIRCLE ( 'NONE', #4116, 9.000000000000000000 ) ;
#8037 = ORIENTED_EDGE ( 'NONE', *, *, #14056, .T. ) ;
#8038 = ORIENTED_EDGE ( 'NONE', *, *, #11603, .T. ) ;
#8039 = ORIENTED_EDGE ( 'NONE', *, *, #5666, .F. ) ;
#8040 = EDGE_CURVE ( 'NONE', #6009, #13255, #8204, .T. ) ;
#8041 = VERTEX_POINT ( 'NONE', #14450 ) ;
#8042 = CARTESIAN_POINT ( 'NONE',  ( 126.5370453525553387, 80.55045718954887946, 49.99999999999999289 ) ) ;
#8043 = ORIENTED_EDGE ( 'NONE', *, *, #15676, .F. ) ;
#8044 = CARTESIAN_POINT ( 'NONE',  ( -67.36461649554505016, 39.84224160888970800, 110.9660488491356887 ) ) ;
#8045 = EDGE_CURVE ( 'NONE', #9731, #20066, #17727, .T. ) ;
#8046 = CARTESIAN_POINT ( 'NONE',  ( -107.4999999999999858, -118.5063289449133777, 40.00000000000000000 ) ) ;
#8047 = CARTESIAN_POINT ( 'NONE',  ( 60.08331549348424971, 8.939227532413909216, 283.5832628385307999 ) ) ;
#8048 = ORIENTED_EDGE ( 'NONE', *, *, #18134, .F. ) ;
#8049 = DIRECTION ( 'NONE',  ( 0.5742676632334713371, -0.8186676071302493307, 0.000000000000000000 ) ) ;
#8050 = DIRECTION ( 'NONE',  ( 1.000000000000000000, 0.000000000000000000, 0.000000000000000000 ) ) ;
#8051 = VECTOR ( 'NONE', #10403, 1000.000000000000000 ) ;
#8052 = VERTEX_POINT ( 'NONE', #11574 ) ;
#8053 = AXIS2_PLACEMENT_3D ( 'NONE', #5658, #8915, #16035 ) ;
#8054 = CYLINDRICAL_SURFACE ( 'NONE', #3490, 7.500000000000008882 ) ;
#8055 = LINE ( 'NONE', #12762, #1936 ) ;
#8056 = FACE_OUTER_BOUND ( 'NONE', #1806, .T. ) ;
#8057 = LINE ( 'NONE', #19120, #11262 ) ;
#8058 = CIRCLE ( 'NONE', #3480, 3.224098631618459443 ) ;
#8059 = CARTESIAN_POINT ( 'NONE',  ( 0.000000000000000000, 0.000000000000000000, -105.0000000000000142 ) ) ;
#8060 = CARTESIAN_POINT ( 'NONE',  ( -29.99999999999887379, 275.0000000000000000, -2.500000000000847766 ) ) ;
#8061 = DIRECTION ( 'NONE',  ( 0.2225209339563182509, -0.9749279121818227312, 0.000000000000000000 ) ) ;
#8062 = ORIENTED_EDGE ( 'NONE', *, *, #14116, .T. ) ;
#8063 = MANIFOLD_SOLID_BREP ( 'BearingFace', #9352 ) ;
#8064 = ORIENTED_EDGE ( 'NONE', *, *, #12348, .F. ) ;
#8065 = ORIENTED_EDGE ( 'NONE', *, *, #11374, .F. ) ;
#8066 = LINE ( 'NONE', #14106, #611 ) ;
#8067 = VERTEX_POINT ( 'NONE', #3704 ) ;
#8068 = FACE_OUTER_BOUND ( 'NONE', #19061, .T. ) ;
#8069 = AXIS2_PLACEMENT_3D ( 'NONE', #6058, #7779, #16891 ) ;
#8070 = FACE_OUTER_BOUND ( 'NONE', #15331, .T. ) ;
#8071 = AXIS2_PLACEMENT_3D ( 'NONE', #14682, #7206, #13425 ) ;
#8072 = EDGE_LOOP ( 'NONE', ( #14392, #2095, #7193, #20203 ) ) ;
#8073 = DIRECTION ( 'NONE',  ( 0.000000000000000000, 0.000000000000000000, 1.000000000000000000 ) ) ;
#8074 = DIRECTION ( 'NONE',  ( 0.000000000000000000, 0.000000000000000000, -1.000000000000000000 ) ) ;
#8075 = CARTESIAN_POINT ( 'NONE',  ( 37.09555676056997697, -45.48770046196272432, 132.4711112102474146 ) ) ;
#8076 = DIRECTION ( 'NONE',  ( 1.000000000000000000, 0.000000000000000000, 0.000000000000000000 ) ) ;
#8077 = DIRECTION ( 'NONE',  ( 0.000000000000000000, 0.000000000000000000, 1.000000000000000000 ) ) ;
#8078 = ORIENTED_EDGE ( 'NONE', *, *, #16389, .F. ) ;
#8079 = CARTESIAN_POINT ( 'NONE',  ( 48.17797692984161984, 36.99387960884179449, 283.5832628385307999 ) ) ;
#8080 = DIRECTION ( 'NONE',  ( -0.000000000000000000, -0.000000000000000000, 1.000000000000000000 ) ) ;
#8081 = CARTESIAN_POINT ( 'NONE',  ( -110.0000000000000142, 275.0000000000000000, 5.000000000000000888 ) ) ;
#8082 = CARTESIAN_POINT ( 'NONE',  ( -27.53920554013687649, -73.25972925305620720, 111.4180192758973931 ) ) ;
#8083 = AXIS2_PLACEMENT_3D ( 'NONE', #13983, #18293, #20226 ) ;
#8084 = ORIENTED_EDGE ( 'NONE', *, *, #10979, .F. ) ;
#8085 = CARTESIAN_POINT ( 'NONE',  ( -109.5721339228235820, 31.03941509555038181, 39.88498244535622206 ) ) ;
#8086 = CARTESIAN_POINT ( 'NONE',  ( 7.950000000000000178, 0.000000000000000000, 0.000000000000000000 ) ) ;
#8087 = VECTOR ( 'NONE', #3732, 1000.000000000000114 ) ;
#8088 = EDGE_LOOP ( 'NONE', ( #9456, #15028, #1830, #11918 ) ) ;
#8089 = VERTEX_POINT ( 'NONE', #14646 ) ;
#8090 = ORIENTED_EDGE ( 'NONE', *, *, #15177, .F. ) ;
#8091 = PRODUCT_CONTEXT ( 'NONE', #3590, 'mechanical' ) ;
#8092 = ORIENTED_EDGE ( 'NONE', *, *, #5362, .F. ) ;
#8093 = ADVANCED_FACE ( 'NONE', ( #8304 ), #14551, .T. ) ;
#8094 = CARTESIAN_POINT ( 'NONE',  ( -98.17232476720997170, -133.0668712321317741, 6.370955715338651792 ) ) ;
#8095 = CARTESIAN_POINT ( 'NONE',  ( -149.9004280568922809, 5.577261304408828835, 7.878901868833741773 ) ) ;
#8096 = ORIENTED_EDGE ( 'NONE', *, *, #7253, .T. ) ;
#8097 =( LENGTH_UNIT ( ) NAMED_UNIT ( * ) SI_UNIT ( .MILLI., .METRE. ) );
#8098 = FACE_BOUND ( 'NONE', #367, .T. ) ;
#8099 = CARTESIAN_POINT ( 'NONE',  ( 128.8937720816053343, -76.72575536401154750, 47.58463383931721324 ) ) ;
#8100 = AXIS2_PLACEMENT_3D ( 'NONE', #7121, #14987, #12950 ) ;
#8101 = VECTOR ( 'NONE', #10796, 1000.000000000000000 ) ;
#8102 = CARTESIAN_POINT ( 'NONE',  ( -91.69714670201400963, -118.7099181436120432, -7.507405155613667169 ) ) ;
#8103 = FACE_BOUND ( 'NONE', #15734, .T. ) ;
#8104 = CARTESIAN_POINT ( 'NONE',  ( -159.9599531637108782, -36.50981547337168109, 60.00000000000000000 ) ) ;
#8105 = ADVANCED_FACE ( 'NONE', ( #2181 ), #6782, .F. ) ;
#8106 = DIRECTION ( 'NONE',  ( 0.6427876096865353661, 0.7660444431189813441, 0.000000000000000000 ) ) ;
#8107 = ADVANCED_FACE ( 'NONE', ( #14352 ), #13098, .F. ) ;
#8108 = CARTESIAN_POINT ( 'NONE',  ( 28.15057869795588985, 51.51682027493075111, 110.9660488491356887 ) ) ;
#8109 = CARTESIAN_POINT ( 'NONE',  ( 127.4413876050234364, 0.000000000000000000, 39.88498244535456649 ) ) ;
#8110 = DIRECTION ( 'NONE',  ( 1.000000000000000000, 0.000000000000000000, 0.000000000000000000 ) ) ;
#8111 = ORIENTED_EDGE ( 'NONE', *, *, #772, .F. ) ;
#8112 = ADVANCED_FACE ( 'NONE', ( #224 ), #12807, .T. ) ;
#8113 = LINE ( 'NONE', #3321, #14461 ) ;
#8114 = CONICAL_SURFACE ( 'NONE', #13019, 34.99999999999997868, 0.7853981633974521648 ) ;
#8115 = CIRCLE ( 'NONE', #1244, 27.50000000000000355 ) ;
#8116 = VECTOR ( 'NONE', #4175, 1000.000000000000000 ) ;
#8117 = CIRCLE ( 'NONE', #19552, 62.91752772691707207 ) ;
#8118 = ORIENTED_EDGE ( 'NONE', *, *, #15585, .F. ) ;
#8119 = EDGE_LOOP ( 'NONE', ( #1600, #16488, #9329, #20196 ) ) ;
#8120 = ADVANCED_FACE ( 'NONE', ( #3503 ), #19646, .F. ) ;
#8121 = ORIENTED_EDGE ( 'NONE', *, *, #11704, .T. ) ;
#8122 = CARTESIAN_POINT ( 'NONE',  ( -144.5247897876143384, -14.68938321827882376, 10.83348343318937523 ) ) ;
#8123 = CARTESIAN_POINT ( 'NONE',  ( -25.99419088092141550, 73.82206860051556419, 111.4180192758973931 ) ) ;
#8124 = DIRECTION ( 'NONE',  ( 0.7660444431189792347, -0.6427876096865379196, 0.000000000000000000 ) ) ;
#8125 = CARTESIAN_POINT ( 'NONE',  ( -159.9599531637108782, -36.50981547337168109, 49.99999999999999289 ) ) ;
#8126 = AXIS2_PLACEMENT_3D ( 'NONE', #12957, #11527, #9995 ) ;
#8127 = VECTOR ( 'NONE', #2546, 1000.000000000000000 ) ;
#8128 = CARTESIAN_POINT ( 'NONE',  ( 12.11787020633414080, 60.78082026081718681, 248.9926560891072143 ) ) ;
#8129 = AXIS2_PLACEMENT_3D ( 'NONE', #14176, #18992, #5180 ) ;
#8130 = LINE ( 'NONE', #14379, #726 ) ;
#8131 = DIRECTION ( 'NONE',  ( 6.982962677686266711E-15, -0.000000000000000000, 1.000000000000000000 ) ) ;
#8132 = EDGE_CURVE ( 'NONE', #14586, #2211, #7268, .T. ) ;
#8133 = DIRECTION ( 'NONE',  ( -6.982962677686266711E-15, 0.000000000000000000, -1.000000000000000000 ) ) ;
#8134 = CARTESIAN_POINT ( 'NONE',  ( 126.5370453525553671, 80.55045718954892209, 60.00000000000000000 ) ) ;
#8135 = EDGE_CURVE ( 'NONE', #4473, #241, #18117, .T. ) ;
#8136 = ORIENTED_EDGE ( 'NONE', *, *, #1276, .T. ) ;
#8137 = PRODUCT_DEFINITION ( 'UNKNOWN', '', #7521, #17854 ) ;
#8138 = CARTESIAN_POINT ( 'NONE',  ( 133.6648977371254148, -68.07564730484348559, 39.79982607272240358 ) ) ;
#8139 = CARTESIAN_POINT ( 'NONE',  ( 134.3942145021295289, -75.36533733386920630, 34.64617282042209467 ) ) ;
#8140 = ORIENTED_EDGE ( 'NONE', *, *, #15528, .T. ) ;
#8141 = VECTOR ( 'NONE', #19465, 1000.000000000000000 ) ;
#8142 = EDGE_LOOP ( 'NONE', ( #907, #15153 ) ) ;
#8143 = VECTOR ( 'NONE', #19352, 1000.000000000000000 ) ;
#8144 = VECTOR ( 'NONE', #17777, 1000.000000000000000 ) ;
#8145 = EDGE_LOOP ( 'NONE', ( #14155, #8488, #7929, #16356 ) ) ;
#8146 = FACE_OUTER_BOUND ( 'NONE', #5454, .T. ) ;
#8147 = ADVANCED_FACE ( 'NONE', ( #15139 ), #4195, .F. ) ;
#8148 = ORIENTED_EDGE ( 'NONE', *, *, #7274, .F. ) ;
#8149 = PLANE ( 'NONE',  #2830 ) ;
#8150 = CARTESIAN_POINT ( 'NONE',  ( -123.8492616149702741, -72.31991210363501921, 0.000000000000000000 ) ) ;
#8151 = CARTESIAN_POINT ( 'NONE',  ( -39.37628763770454299, -49.07263256785938665, 248.9926560891072143 ) ) ;
#8152 = CARTESIAN_POINT ( 'NONE',  ( 156.4179374840099683, -52.02840013023883614, 49.99999999999999289 ) ) ;
#8153 = ORIENTED_EDGE ( 'NONE', *, *, #14975, .F. ) ;
#8154 = CARTESIAN_POINT ( 'NONE',  ( -189.9999999999988916, 265.0000000000000000, 5.000000000000268230 ) ) ;
#8155 = CARTESIAN_POINT ( 'NONE',  ( 51.77251465595239921, -31.77296517111717478, 283.5832628385307999 ) ) ;
#8156 = VERTEX_POINT ( 'NONE', #2469 ) ;
#8157 = CARTESIAN_POINT ( 'NONE',  ( 44.07268132743672595, 38.78191089773085309, 132.4711112102474146 ) ) ;
#8158 = DIRECTION ( 'NONE',  ( -0.000000000000000000, -0.000000000000000000, 1.000000000000000000 ) ) ;
#8159 = ADVANCED_FACE ( 'NONE', ( #13191 ), #16584, .T. ) ;
#8160 = FACE_OUTER_BOUND ( 'NONE', #4059, .T. ) ;
#8161 = AXIS2_PLACEMENT_3D ( 'NONE', #18209, #16581, #7458 ) ;
#8162 = AXIS2_PLACEMENT_3D ( 'NONE', #8125, #2101, #5076 ) ;
#8163 = ADVANCED_FACE ( 'NONE', ( #19457 ), #3394, .F. ) ;
#8164 = EDGE_CURVE ( 'NONE', #18256, #9985, #2468, .T. ) ;
#8165 = DIRECTION ( 'NONE',  ( 0.8660254037844363761, 0.5000000000000039968, 0.000000000000000000 ) ) ;
#8166 = DIRECTION ( 'NONE',  ( 0.3088643371590157338, -0.9511061040868794558, 0.000000000000000000 ) ) ;
#8167 = CARTESIAN_POINT ( 'NONE',  ( 82.03125000000004263, -125.5821405433013780, 30.00000000000000000 ) ) ;
#8168 = EDGE_CURVE ( 'NONE', #4702, #14818, #2772, .T. ) ;
#8169 = ORIENTED_EDGE ( 'NONE', *, *, #12501, .T. ) ;
#8170 = DIRECTION ( 'NONE',  ( -0.000000000000000000, -1.000000000000000000, -0.000000000000000000 ) ) ;
#8171 = ORIENTED_EDGE ( 'NONE', *, *, #763, .F. ) ;
#8172 = ORIENTED_EDGE ( 'NONE', *, *, #1201, .F. ) ;
#8173 = CARTESIAN_POINT ( 'NONE',  ( -14.02132266220276691, 20.55229278271246329, 14.88498244535555060 ) ) ;
#8174 =( GEOMETRIC_REPRESENTATION_CONTEXT ( 3 ) GLOBAL_UNCERTAINTY_ASSIGNED_CONTEXT ( ( #81 ) ) GLOBAL_UNIT_ASSIGNED_CONTEXT ( ( #12072, #11974, #1139 ) ) REPRESENTATION_CONTEXT ( 'NONE', 'WORKASPACE' ) );
#8175 = VERTEX_POINT ( 'NONE', #8995 ) ;
#8176 = CIRCLE ( 'NONE', #1980, 106.4288957539801004 ) ;
#8177 = DIRECTION ( 'NONE',  ( 0.000000000000000000, 0.000000000000000000, 1.000000000000000000 ) ) ;
#8178 = CARTESIAN_POINT ( 'NONE',  ( 0.000000000000000000, 0.000000000000000000, 283.5832628385307999 ) ) ;
#8179 = ORIENTED_EDGE ( 'NONE', *, *, #5124, .T. ) ;
#8180 = LINE ( 'NONE', #5316, #173 ) ;
#8181 = LINE ( 'NONE', #14427, #10168 ) ;
#8182 = DIRECTION ( 'NONE',  ( 1.613511099790691498E-16, -1.000000000000000000, 0.000000000000000000 ) ) ;
#8183 = DIRECTION ( 'NONE',  ( -1.000000000000000000, 0.000000000000000000, 0.000000000000000000 ) ) ;
#8184 = DIRECTION ( 'NONE',  ( 0.4999999999999919509, -0.8660254037844432595, -3.488592933436654014E-15 ) ) ;
#8185 = ORIENTED_EDGE ( 'NONE', *, *, #3358, .T. ) ;
#8186 = CARTESIAN_POINT ( 'NONE',  ( 38.78191089773071809, -44.07268132743684674, 110.7293897666001214 ) ) ;
#8187 = CARTESIAN_POINT ( 'NONE',  ( 0.000000000000000000, 0.000000000000000000, 293.5832628385307999 ) ) ;
#8188 = PLANE ( 'NONE',  #16672 ) ;
#8189 = VECTOR ( 'NONE', #6460, 999.9999999999998863 ) ;
#8190 = CARTESIAN_POINT ( 'NONE',  ( -73.06915264522022824, -28.06281046684250313, 132.4711112102474146 ) ) ;
#8191 = VERTEX_POINT ( 'NONE', #5947 ) ;
#8192 = LINE ( 'NONE', #16079, #4864 ) ;
#8193 = CARTESIAN_POINT ( 'NONE',  ( -78.11514653572207578, 128.0610818020408601, 29.21201989692128365 ) ) ;
#8194 = EDGE_LOOP ( 'NONE', ( #13403, #13131 ) ) ;
#8195 = ORIENTED_EDGE ( 'NONE', *, *, #2474, .T. ) ;
#8196 = ORIENTED_EDGE ( 'NONE', *, *, #6857, .F. ) ;
#8197 = PRODUCT_CONTEXT ( 'NONE', #1885, 'mechanical' ) ;
#8198 = ORIENTED_EDGE ( 'NONE', *, *, #16363, .F. ) ;
#8199 = AXIS2_PLACEMENT_3D ( 'NONE', #19318, #5400, #11529 ) ;
#8200 = DIRECTION ( 'NONE',  ( 1.000000000000000000, 0.000000000000000000, 0.000000000000000000 ) ) ;
#8201 = MANIFOLD_SOLID_BREP ( 'CirPattern4', #11315 ) ;
#8202 = ORIENTED_EDGE ( 'NONE', *, *, #18273, .T. ) ;
#8203 = AXIS2_PLACEMENT_3D ( 'NONE', #7205, #16424, #8831 ) ;
#8204 = LINE ( 'NONE', #5344, #445 ) ;
#8205 = DIRECTION ( 'NONE',  ( 0.000000000000000000, 0.000000000000000000, 1.000000000000000000 ) ) ;
#8206 = CARTESIAN_POINT ( 'NONE',  ( -96.82170812967324025, -114.6249810635578541, 3.420849988137867559 ) ) ;
#8207 = CARTESIAN_POINT ( 'NONE',  ( -112.4702966502606643, 83.46484221923026325, 39.99999999999999289 ) ) ;
#8208 = VECTOR ( 'NONE', #13014, 1000.000000000000000 ) ;
#8209 = CARTESIAN_POINT ( 'NONE',  ( -51.36153797460868731, 59.06449708980214552, 248.9926560891072143 ) ) ;
#8210 = DIRECTION ( 'NONE',  ( 0.9749279121818261729, -0.2225209339563031519, 0.000000000000000000 ) ) ;
#8211 = DIRECTION ( 'NONE',  ( 0.8660254037844450359, -0.4999999999999889533, 0.000000000000000000 ) ) ;
#8212 = DIRECTION ( 'NONE',  ( -0.000000000000000000, -0.000000000000000000, -1.000000000000000000 ) ) ;
#8213 = LINE ( 'NONE', #17835, #9318 ) ;
#8214 = EDGE_CURVE ( 'NONE', #1847, #15721, #12163, .T. ) ;
#8215 = ORIENTED_EDGE ( 'NONE', *, *, #4775, .T. ) ;
#8216 = DIRECTION ( 'NONE',  ( -0.000000000000000000, -0.000000000000000000, 1.000000000000000000 ) ) ;
#8217 = ORIENTED_EDGE ( 'NONE', *, *, #12979, .F. ) ;
#8218 = ORIENTED_EDGE ( 'NONE', *, *, #3733, .F. ) ;
#8219 = EDGE_CURVE ( 'NONE', #19500, #6948, #19140, .T. ) ;
#8220 = ORIENTED_EDGE ( 'NONE', *, *, #2499, .F. ) ;
#8221 = LINE ( 'NONE', #11686, #6990 ) ;
#8222 = EDGE_CURVE ( 'NONE', #7430, #934, #1949, .T. ) ;
#8223 = CARTESIAN_POINT ( 'NONE',  ( -135.1060089022256818, -65.16414933467417825, 10.00000000000000178 ) ) ;
#8224 = CARTESIAN_POINT ( 'NONE',  ( 5.590028426173794251, 1.289614712049196976, 283.5832628385307999 ) ) ;
#8225 = CARTESIAN_POINT ( 'NONE',  ( -7.499999999999583444, -60.00000000000000000, -105.0000000000000142 ) ) ;
#8226 = LINE ( 'NONE', #11093, #10393 ) ;
#8227 = CARTESIAN_POINT ( 'NONE',  ( -7.500000000000001776, 60.00000000000000000, -100.0000000000000000 ) ) ;
#8228 = MANIFOLD_SOLID_BREP ( 'Chamfer2', #862 ) ;
#8229 = CARTESIAN_POINT ( 'NONE',  ( 0.000000000000000000, 0.000000000000000000, 283.5832628385307999 ) ) ;
#8230 = VECTOR ( 'NONE', #8210, 1000.000000000000114 ) ;
#8231 = DIRECTION ( 'NONE',  ( 0.000000000000000000, 0.000000000000000000, 1.000000000000000000 ) ) ;
#8232 = CARTESIAN_POINT ( 'NONE',  ( 0.000000000000000000, 0.000000000000000000, 293.5832628385307999 ) ) ;
#8233 = EDGE_CURVE ( 'NONE', #2918, #7528, #6560, .T. ) ;
#8234 = ORIENTED_EDGE ( 'NONE', *, *, #5529, .F. ) ;
#8235 = DIRECTION ( 'NONE',  ( 0.000000000000000000, 0.000000000000000000, -1.000000000000000000 ) ) ;
#8236 = ORIENTED_EDGE ( 'NONE', *, *, #8607, .F. ) ;
#8237 = VERTEX_POINT ( 'NONE', #12881 ) ;
#8238 = ORIENTED_EDGE ( 'NONE', *, *, #6045, .F. ) ;
#8239 = ORIENTED_EDGE ( 'NONE', *, *, #6286, .T. ) ;
#8240 = LINE ( 'NONE', #12944, #6339 ) ;
#8241 = ADVANCED_FACE ( 'NONE', ( #3580 ), #19332, .T. ) ;
#8242 = VECTOR ( 'NONE', #5261, 1000.000000000000000 ) ;
#8243 = VECTOR ( 'NONE', #18738, 1000.000000000000000 ) ;
#8244 = ORIENTED_EDGE ( 'NONE', *, *, #7214, .T. ) ;
#8245 = CARTESIAN_POINT ( 'NONE',  ( -23.22641211976288389, -56.12662799072081299, 283.5832628385307999 ) ) ;
#8246 = EDGE_CURVE ( 'NONE', #12149, #3301, #14736, .T. ) ;
#8247 = CARTESIAN_POINT ( 'NONE',  ( -102.1674435767773019, -127.3754966267598121, 38.48120063021033843 ) ) ;
#8248 = LINE ( 'NONE', #14195, #17254 ) ;
#8249 = ORIENTED_EDGE ( 'NONE', *, *, #1870, .F. ) ;
#8250 = AXIS2_PLACEMENT_3D ( 'NONE', #13277, #5724, #11840 ) ;
#8251 = CARTESIAN_POINT ( 'NONE',  ( 134.2425157119613459, -66.92593549375909845, 2.347053091275800973 ) ) ;
#8252 = DIRECTION ( 'NONE',  ( 0.000000000000000000, 0.000000000000000000, -1.000000000000000000 ) ) ;
#8253 = VERTEX_POINT ( 'NONE', #14716 ) ;
#8254 = CARTESIAN_POINT ( 'NONE',  ( 59.06449708980163393, 51.36153797460926995, 110.7293897666001214 ) ) ;
#8255 = DIRECTION ( 'NONE',  ( -0.1736481776669374644, 0.9848077530122069101, 0.000000000000000000 ) ) ;
#8256 = LINE ( 'NONE', #14505, #13408 ) ;
#8257 = FACE_OUTER_BOUND ( 'NONE', #11445, .T. ) ;
#8258 = ADVANCED_FACE ( 'NONE', ( #897 ), #5421, .F. ) ;
#8259 = AXIS2_PLACEMENT_3D ( 'NONE', #10951, #7476, #12176 ) ;
#8260 = AXIS2_PLACEMENT_3D ( 'NONE', #7896, #11067, #12396 ) ;
#8261 = CARTESIAN_POINT ( 'NONE',  ( -141.1002642289847131, -19.56295509475995686, -11.10155280223196961 ) ) ;
#8262 = CARTESIAN_POINT ( 'NONE',  ( 0.000000000000000000, 0.000000000000000000, 132.4711112102474146 ) ) ;
#8263 = CARTESIAN_POINT ( 'NONE',  ( -6.191009641800430785, -26.42934155884822900, 14.88498244535549375 ) ) ;
#8264 = ORIENTED_EDGE ( 'NONE', *, *, #2272, .T. ) ;
#8265 = DIRECTION ( 'NONE',  ( -1.000000000000000000, 0.000000000000000000, 0.000000000000000000 ) ) ;
#8266 = VERTEX_POINT ( 'NONE', #18091 ) ;
#8267 = AXIS2_PLACEMENT_3D ( 'NONE', #4573, #4988, #12541 ) ;
#8268 = ORIENTED_EDGE ( 'NONE', *, *, #2547, .T. ) ;
#8269 = DIRECTION ( 'NONE',  ( -0.000000000000000000, -0.000000000000000000, 1.000000000000000000 ) ) ;
#8270 = CIRCLE ( 'NONE', #7945, 60.74260934110282051 ) ;
#8271 = ORIENTED_EDGE ( 'NONE', *, *, #17109, .F. ) ;
#8272 = EDGE_CURVE ( 'NONE', #3178, #20227, #13366, .T. ) ;
#8273 = ADVANCED_FACE ( 'NONE', ( #800, #13167, #7049, #7339, #8478, #10015 ), #11826, .F. ) ;
#8274 = EDGE_CURVE ( 'NONE', #4648, #20212, #3873, .T. ) ;
#8275 = EDGE_CURVE ( 'NONE', #8865, #10778, #4066, .T. ) ;
#8276 = CARTESIAN_POINT ( 'NONE',  ( -107.4999999999999716, -200.0000000000000000, 40.00000000000000000 ) ) ;
#8277 = CARTESIAN_POINT ( 'NONE',  ( 27.50000000000001776, 3.367778697655222096E-15, 127.7817459305202448 ) ) ;
#8278 = CIRCLE ( 'NONE', #2086, 112.8770930172170637 ) ;
#8279 = DIRECTION ( 'NONE',  ( 0.8186676071302501079, -0.5742676632334704490, 0.000000000000000000 ) ) ;
#8280 = CARTESIAN_POINT ( 'NONE',  ( 156.4179374840099683, -52.02840013023883614, 60.00000000000000000 ) ) ;
#8281 = CARTESIAN_POINT ( 'NONE',  ( 1.396592535537253342E-14, 0.000000000000000000, 49.99999999999999289 ) ) ;
#8282 = VECTOR ( 'NONE', #271, 1000.000000000000114 ) ;
#8283 = DIRECTION ( 'NONE',  ( -0.000000000000000000, -0.000000000000000000, 1.000000000000000000 ) ) ;
#8284 = DIRECTION ( 'NONE',  ( -0.3747554100459928317, -0.9271237148521548344, 0.000000000000000000 ) ) ;
#8285 = FACE_OUTER_BOUND ( 'NONE', #14544, .T. ) ;
#8286 = ADVANCED_FACE ( 'NONE', ( #14816 ), #703, .F. ) ;
#8287 = CARTESIAN_POINT ( 'NONE',  ( 0.000000000000000000, 0.000000000000000000, 248.9926560891072143 ) ) ;
#8288 = LINE ( 'NONE', #12477, #1320 ) ;
#8289 = CARTESIAN_POINT ( 'NONE',  ( 96.22303100968534295, -115.1714777947412074, 35.55703238301298796 ) ) ;
#8290 = VERTEX_POINT ( 'NONE', #11642 ) ;
#8291 = DIRECTION ( 'NONE',  ( 6.982962677686266711E-15, -0.000000000000000000, 1.000000000000000000 ) ) ;
#8292 = CARTESIAN_POINT ( 'NONE',  ( -71.68195843679204415, 131.7647605457766815, -6.617816534668000905 ) ) ;
#8293 = EDGE_LOOP ( 'NONE', ( #9630, #13559, #887, #18637 ) ) ;
#8294 = ORIENTED_EDGE ( 'NONE', *, *, #8997, .F. ) ;
#8295 = ORIENTED_EDGE ( 'NONE', *, *, #11291, .F. ) ;
#8296 = ITEM_DEFINED_TRANSFORMATION ( 'NONE', 'NONE', #5252,  #18639 ) ;
#8297 = EDGE_CURVE ( 'NONE', #14124, #6346, #10301, .T. ) ;
#8298 = CIRCLE ( 'NONE', #9276, 60.74260934110282051 ) ;
#8299 = ORIENTED_EDGE ( 'NONE', *, *, #19128, .F. ) ;
#8300 = PLANE ( 'NONE',  #14687 ) ;
#8301 = CARTESIAN_POINT ( 'NONE',  ( -122.5362376193369442, 86.52404603474892042, 42.99233187391926947 ) ) ;
#8302 = AXIS2_PLACEMENT_3D ( 'NONE', #2321, #16134, #17680 ) ;
#8303 = ORIENTED_EDGE ( 'NONE', *, *, #15198, .T. ) ;
#8304 = FACE_OUTER_BOUND ( 'NONE', #19158, .T. ) ;
#8305 = DIRECTION ( 'NONE',  ( 0.000000000000000000, 0.000000000000000000, 1.000000000000000000 ) ) ;
#8306 = CARTESIAN_POINT ( 'NONE',  ( -84.12422660803102303, -124.1903156958427559, 0.7897671010553509729 ) ) ;
#8307 = VERTEX_POINT ( 'NONE', #19817 ) ;
#8308 = EDGE_CURVE ( 'NONE', #16337, #3938, #1828, .T. ) ;
#8309 = DIRECTION ( 'NONE',  ( -3.491481338843133355E-15, 1.000000000000000000, 0.000000000000000000 ) ) ;
#8310 = DIRECTION ( 'NONE',  ( 0.2225209339563182231, -0.9749279121818227312, 0.000000000000000000 ) ) ;
#8311 = AXIS2_PLACEMENT_3D ( 'NONE', #17092, #1648, #17202 ) ;
#8312 = PLANE ( 'NONE',  #9141 ) ;
#8313 = CARTESIAN_POINT ( 'NONE',  ( 37.93579148621461883, 68.46530598706807780, 110.9660488491356887 ) ) ;
#8314 = DIRECTION ( 'NONE',  ( -0.000000000000000000, -0.000000000000000000, 1.000000000000000000 ) ) ;
#8315 = ORIENTED_EDGE ( 'NONE', *, *, #7836, .F. ) ;
#8316 = CARTESIAN_POINT ( 'NONE',  ( -130.0921664654442509, 42.14112310077317858, -23.71395948546228283 ) ) ;
#8317 = AXIS2_PLACEMENT_3D ( 'NONE', #14571, #3723, #7098 ) ;
#8318 = ORIENTED_EDGE ( 'NONE', *, *, #16234, .T. ) ;
#8319 = VECTOR ( 'NONE', #16585, 1000.000000000000000 ) ;
#8320 = ORIENTED_EDGE ( 'NONE', *, *, #18557, .F. ) ;
#8321 = EDGE_LOOP ( 'NONE', ( #16060, #454, #8813, #8568 ) ) ;
#8322 = AXIS2_PLACEMENT_3D ( 'NONE', #19220, #8165, #15740 ) ;
#8323 = LINE ( 'NONE', #14569, #3064 ) ;
#8324 = ADVANCED_FACE ( 'NONE', ( #16562 ), #2542, .T. ) ;
#8325 = DIRECTION ( 'NONE',  ( 0.000000000000000000, 1.000000000000000000, 0.000000000000000000 ) ) ;
#8326 = DIRECTION ( 'NONE',  ( 0.000000000000000000, 1.000000000000000000, 0.000000000000000000 ) ) ;
#8327 = CARTESIAN_POINT ( 'NONE',  ( -50.93469132750304595, -59.42266395395772349, 132.4711112102474146 ) ) ;
#8328 = CARTESIAN_POINT ( 'NONE',  ( 0.000000000000000000, 0.000000000000000000, 293.5832628385307999 ) ) ;
#8329 = CARTESIAN_POINT ( 'NONE',  ( -3.221721112346616067, 26.95290724009910832, 14.88498244535547244 ) ) ;
#8330 = CARTESIAN_POINT ( 'NONE',  ( 50.93469132750264095, 59.42266395395811429, 248.9926560891072143 ) ) ;
#8331 = DIRECTION ( 'NONE',  ( 1.000000000000000000, 0.000000000000000000, 0.000000000000000000 ) ) ;
#8332 = VECTOR ( 'NONE', #11827, 1000.000000000000000 ) ;
#8333 = CARTESIAN_POINT ( 'NONE',  ( 60.00000000000000711, 6.284666409917639535E-13, -105.0000000000000142 ) ) ;
#8334 = EDGE_LOOP ( 'NONE', ( #2680, #8692, #10949, #18153 ) ) ;
#8335 = EDGE_CURVE ( 'NONE', #18849, #12537, #12590, .T. ) ;
#8336 = CIRCLE ( 'NONE', #3121, 62.91752772691707207 ) ;
#8337 = ORIENTED_EDGE ( 'NONE', *, *, #745, .T. ) ;
#8338 =( BOUNDED_SURFACE ( )  B_SPLINE_SURFACE ( 3, 2, ( 
 ( #3828, #19675, #5671 ),
 ( #14965, #14679, #3928 ),
 ( #16420, #10071, #7005 ),
 ( #16323, #13035, #664 ),
 ( #6910, #2307, #14770 ),
 ( #855, #15069, #954 ),
 ( #11886, #5467, #11789 ),
 ( #10169, #2403, #4126 ),
 ( #5568, #18050, #7204 ),
 ( #6809, #11988, #4433 ),
 ( #9030, #5876, #1366 ),
 ( #1260, #3009, #7594 ),
 ( #12300, #16918, #18451 ),
 ( #10663, #15272, #5975 ),
 ( #16713, #7395, #2698 ),
 ( #2906, #20081, #7498 ),
 ( #2806, #13734, #4324 ),
 ( #19978, #1154, #6080 ),
 ( #13630, #19874, #8927 ),
 ( #15376, #17023, #18556 ),
 ( #13836, #10868, #4538 ),
 ( #9239, #12197, #17124 ),
 ( #9135, #1468, #10770 ),
 ( #15483, #13526, #9342 ),
 ( #7698, #19775, #15171 ),
 ( #13941, #20186, #12089 ),
 ( #18349, #6187, #10558 ),
 ( #16814, #12407, #18667 ),
 ( #4644, #3112, #1048 ),
 ( #5773, #7297, #18243 ) ),
 .UNSPECIFIED., .F., .F., .F. ) 
 B_SPLINE_SURFACE_WITH_KNOTS ( ( 4, 2, 2, 2, 2, 2, 2, 2, 2, 2, 2, 2, 2, 2, 4 ),
 ( 3, 3 ),
 ( 0.01087485647533276839, 0.01538493460406631201, 0.01651245413624969835, 0.01763997366843308295, 0.01989501273279985563, 0.02102253226498324024, 0.02215005179716662831, 0.02440509086153339752, 0.02891516899026694287, 0.03117020805463371555, 0.03342524711900048823, 0.03793532524773403358, 0.04019036431210080279, 0.04244540337646757200, 0.04695548150520111735 ),
 ( 0.000000000000000000, 1.000000000000000000 ),
 .UNSPECIFIED. ) 
 GEOMETRIC_REPRESENTATION_ITEM ( )  RATIONAL_B_SPLINE_SURFACE ( (
 ( 1.000000000000000000, 0.9212076576725561905, 1.000000000000000000),
 ( 1.000000000000000000, 0.9211983545445133759, 1.000000000000000000),
 ( 1.000000000000000000, 0.9192884530627715156, 1.000000000000000000),
 ( 1.000000000000000000, 0.9147257148663896498, 1.000000000000000000),
 ( 1.000000000000000000, 0.9137002753876459771, 1.000000000000000000),
 ( 1.000000000000000000, 0.9114460110779207813, 1.000000000000000000),
 ( 1.000000000000000000, 0.9102239901659180399, 1.000000000000000000),
 ( 1.000000000000000000, 0.9062907615862647592, 1.000000000000000000),
 ( 1.000000000000000000, 0.9033134084428577903, 1.000000000000000000),
 ( 1.000000000000000000, 0.8983619464026604273, 1.000000000000000000),
 ( 1.000000000000000000, 0.8966302762932976123, 1.000000000000000000),
 ( 1.000000000000000000, 0.8930095736512202453, 1.000000000000000000),
 ( 1.000000000000000000, 0.8911146393079001360, 1.000000000000000000),
 ( 1.000000000000000000, 0.8852539528818137438, 1.000000000000000000),
 ( 1.000000000000000000, 0.8811119717501193493, 1.000000000000000000),
 ( 1.000000000000000000, 0.8680569459630019802, 1.000000000000000000),
 ( 1.000000000000000000, 0.8585210289498550473, 1.000000000000000000),
 ( 1.000000000000000000, 0.8431029601255768391, 1.000000000000000000),
 ( 1.000000000000000000, 0.8377859708360378965, 1.000000000000000000),
 ( 1.000000000000000000, 0.8269824639698531987, 1.000000000000000000),
 ( 1.000000000000000000, 0.8214732595402479687, 1.000000000000000000),
 ( 1.000000000000000000, 0.8046428831056189335, 1.000000000000000000),
 ( 1.000000000000000000, 0.7930208592508356524, 1.000000000000000000),
 ( 1.000000000000000000, 0.7750195416464756848, 1.000000000000000000),
 ( 1.000000000000000000, 0.7688986879967366628, 1.000000000000000000),
 ( 1.000000000000000000, 0.7566232400043410022, 1.000000000000000000),
 ( 1.000000000000000000, 0.7504663834241424025, 1.000000000000000000),
 ( 1.000000000000000000, 0.7319497228655966747, 1.000000000000000000),
 ( 1.000000000000000000, 0.7195437534944766345, 1.000000000000000000),
 ( 1.000000000000000000, 0.7071067811865472397, 1.000000000000000000) ) ) 
 REPRESENTATION_ITEM ( '' )  SURFACE ( )  );
#8339 = ORIENTED_EDGE ( 'NONE', *, *, #2361, .T. ) ;
#8340 = ORIENTED_EDGE ( 'NONE', *, *, #6415, .T. ) ;
#8341 = EDGE_LOOP ( 'NONE', ( #5456, #2078, #4944 ) ) ;
#8342 = VERTEX_POINT ( 'NONE', #15015 ) ;
#8343 = AXIS2_PLACEMENT_3D ( 'NONE', #3992, #6972, #11855 ) ;
#8344 = LINE ( 'NONE', #10085, #2404 ) ;
#8345 = ADVANCED_FACE ( 'NONE', ( #996 ), #10115, .T. ) ;
#8346 = CARTESIAN_POINT ( 'NONE',  ( -20.74471755083563806, 59.39925916207565137, 293.5832628385307999 ) ) ;
#8347 = EDGE_CURVE ( 'NONE', #7001, #17581, #5712, .T. ) ;
#8348 = DIRECTION ( 'NONE',  ( 0.000000000000000000, -0.000000000000000000, 1.000000000000000000 ) ) ;
#8349 = DIRECTION ( 'NONE',  ( 0.000000000000000000, 0.000000000000000000, 1.000000000000000000 ) ) ;
#8350 = ORIENTED_EDGE ( 'NONE', *, *, #10008, .T. ) ;
#8351 = CARTESIAN_POINT ( 'NONE',  ( 133.9144309718294608, -67.58001956112548214, 1.097951290815503356 ) ) ;
#8352 = LINE ( 'NONE', #9689, #5857 ) ;
#8353 = ORIENTED_EDGE ( 'NONE', *, *, #1850, .T. ) ;
#8354 = DIRECTION ( 'NONE',  ( 1.000000000000000000, 0.000000000000000000, 0.000000000000000000 ) ) ;
#8355 = DIRECTION ( 'NONE',  ( -0.9848077530122067991, -0.1736481776669374366, 0.000000000000000000 ) ) ;
#8356 = CARTESIAN_POINT ( 'NONE',  ( 159.9599531637113330, -36.50981547336952104, 60.00000000000000000 ) ) ;
#8357 = VECTOR ( 'NONE', #20009, 1000.000000000000000 ) ;
#8358 = DIRECTION ( 'NONE',  ( 1.000000000000000000, 0.000000000000000000, 0.000000000000000000 ) ) ;
#8359 = EDGE_CURVE ( 'NONE', #5887, #19198, #9663, .T. ) ;
#8360 = EDGE_CURVE ( 'NONE', #10908, #5623, #15110, .T. ) ;
#8361 = PLANE ( 'NONE',  #9723 ) ;
#8362 = LINE ( 'NONE', #14803, #16740 ) ;
#8363 = CARTESIAN_POINT ( 'NONE',  ( -78.37722339831623231, 116.0043570404596522, -9.999999999999984013 ) ) ;
#8364 = ORIENTED_EDGE ( 'NONE', *, *, #6918, .F. ) ;
#8365 = EDGE_CURVE ( 'NONE', #17410, #5784, #3770, .T. ) ;
#8366 = AXIS2_PLACEMENT_3D ( 'NONE', #8154, #14301, #9789 ) ;
#8367 = CARTESIAN_POINT ( 'NONE',  ( 0.000000000000000000, -3.004629197474319246E-15, -9.000000000000000000 ) ) ;
#8368 = ORIENTED_EDGE ( 'NONE', *, *, #3616, .F. ) ;
#8369 = ORIENTED_EDGE ( 'NONE', *, *, #10212, .F. ) ;
#8370 = DIRECTION ( 'NONE',  ( 0.000000000000000000, 0.000000000000000000, 1.000000000000000000 ) ) ;
#8371 = VERTEX_POINT ( 'NONE', #9390 ) ;
#8372 = AXIS2_PLACEMENT_3D ( 'NONE', #17954, #13314, #3923 ) ;
#8373 = EDGE_CURVE ( 'NONE', #1151, #15881, #3464, .T. ) ;
#8374 = DIRECTION ( 'NONE',  ( 0.000000000000000000, 0.000000000000000000, 1.000000000000000000 ) ) ;
#8375 = AXIS2_PLACEMENT_3D ( 'NONE', #11212, #9585, #9282 ) ;
#8376 = DIRECTION ( 'NONE',  ( -0.7881095627315619634, -0.6155349844899687950, 0.000000000000000000 ) ) ;
#8377 = DIRECTION ( 'NONE',  ( -0.000000000000000000, 0.000000000000000000, -1.000000000000000000 ) ) ;
#8378 = LINE ( 'NONE', #308, #7548 ) ;
#8379 = AXIS2_PLACEMENT_3D ( 'NONE', #12534, #470, #17669 ) ;
#8380 = DIRECTION ( 'NONE',  ( 6.982962677686266711E-15, -0.000000000000000000, 1.000000000000000000 ) ) ;
#8381 = CARTESIAN_POINT ( 'NONE',  ( 97.83396368271631616, -133.5156904852159983, 7.427229934397163724 ) ) ;
#8382 = CARTESIAN_POINT ( 'NONE',  ( -58.03804081968160489, 8.833100819208169696, 112.0427633081292385 ) ) ;
#8383 = CARTESIAN_POINT ( 'NONE',  ( 144.1130761623740568, -69.50842595698583182, 10.00000000000000178 ) ) ;
#8384 = ORIENTED_EDGE ( 'NONE', *, *, #8863, .F. ) ;
#8385 = DIRECTION ( 'NONE',  ( -1.000000000000000000, 0.000000000000000000, 0.000000000000000000 ) ) ;
#8386 = DIRECTION ( 'NONE',  ( 0.000000000000000000, 0.000000000000000000, 1.000000000000000000 ) ) ;
#8387 = EDGE_CURVE ( 'NONE', #3256, #9877, #1412, .T. ) ;
#8388 = CARTESIAN_POINT ( 'NONE',  ( 62.09913334491123749, 10.11498556985180031, 293.5832628385307999 ) ) ;
#8389 = FACE_BOUND ( 'NONE', #2479, .T. ) ;
#8391 = EDGE_CURVE ( 'NONE', #4335, #8743, #7439, .T. ) ;
#8390 = VECTOR ( 'NONE', #1821, 1000.000000000000000 ) ;
#8392 = ORIENTED_EDGE ( 'NONE', *, *, #4656, .T. ) ;
#8393 = EDGE_CURVE ( 'NONE', #2297, #19280, #1513, .T. ) ;
#8394 = PRODUCT_DEFINITION ( 'UNKNOWN', '', #2021, #10918 ) ;
#8395 = AXIS2_PLACEMENT_3D ( 'NONE', #13096, #7073, #4192 ) ;
#8396 = CARTESIAN_POINT ( 'NONE',  ( 40.28046525994349736, 45.46865632508086463, 293.5832628385307999 ) ) ;
#8397 = DIRECTION ( 'NONE',  ( 0.000000000000000000, 0.000000000000000000, -1.000000000000000000 ) ) ;
#8398 = ORIENTED_EDGE ( 'NONE', *, *, #18811, .T. ) ;
#8399 = ORIENTED_EDGE ( 'NONE', *, *, #3897, .T. ) ;
#8401 = ORIENTED_EDGE ( 'NONE', *, *, #3412, .T. ) ;
#8400 = CIRCLE ( 'NONE', #4140, 150.0000000000000284 ) ;
#8402 = APPLICATION_PROTOCOL_DEFINITION ( 'draft international standard', 'automotive_design', 1998, #14040 ) ;
#8403 = CARTESIAN_POINT ( 'NONE',  ( 60.08331549348424971, 8.939227532413909216, 293.5832628385307999 ) ) ;
#8404 = EDGE_CURVE ( 'NONE', #5478, #18696, #18295, .T. ) ;
#8405 = DIRECTION ( 'NONE',  ( 0.000000000000000000, 0.000000000000000000, -1.000000000000000000 ) ) ;
#8406 = ORIENTED_EDGE ( 'NONE', *, *, #4093, .T. ) ;
#8407 = CARTESIAN_POINT ( 'NONE',  ( -163.5019688434124419, -20.99123081650240863, 49.99999999999999289 ) ) ;
#8408 = CARTESIAN_POINT ( 'NONE',  ( -98.61625419099686951, -132.4696700755308996, 5.394883550556022200 ) ) ;
#8409 = ORIENTED_EDGE ( 'NONE', *, *, #16057, .T. ) ;
#8410 = CARTESIAN_POINT ( 'NONE',  ( -82.03125000000001421, -125.5821405433014348, 8.545780905957366613 ) ) ;
#8411 = CARTESIAN_POINT ( 'NONE',  ( 45.46865632508072963, -40.28046525994365368, 293.5832628385307999 ) ) ;
#8412 = VECTOR ( 'NONE', #10101, 1000.000000000000000 ) ;
#8413 = LINE ( 'NONE', #6980, #6306 ) ;
#8414 = EDGE_CURVE ( 'NONE', #4682, #10750, #7700, .T. ) ;
#8415 = EDGE_CURVE ( 'NONE', #2269, #12253, #1195, .T. ) ;
#8416 = CARTESIAN_POINT ( 'NONE',  ( 0.000000000000000000, 0.000000000000000000, 0.000000000000000000 ) ) ;
#8417 = CARTESIAN_POINT ( 'NONE',  ( 0.000000000000000000, 0.000000000000000000, 39.99999999999999289 ) ) ;
#8418 = DIRECTION ( 'NONE',  ( 1.000000000000000000, 0.000000000000000000, 0.000000000000000000 ) ) ;
#8419 = ORIENTED_EDGE ( 'NONE', *, *, #9225, .T. ) ;
#8420 = EDGE_CURVE ( 'NONE', #12185, #11142, #2483, .T. ) ;
#8421 = CARTESIAN_POINT ( 'NONE',  ( -139.6549061548003579, 6.995471948008744612, -13.59954962453111094 ) ) ;
#8422 = ADVANCED_FACE ( 'NONE', ( #1310 ), #13677, .F. ) ;
#8423 = ORIENTED_EDGE ( 'NONE', *, *, #14219, .F. ) ;
#8424 = AXIS2_PLACEMENT_3D ( 'NONE', #10913, #379, #9491 ) ;
#8425 = ORIENTED_EDGE ( 'NONE', *, *, #17504, .F. ) ;
#8426 = CIRCLE ( 'NONE', #5171, 3.224098631618460331 ) ;
#8427 = ORIENTED_EDGE ( 'NONE', *, *, #7785, .F. ) ;
#8428 = CARTESIAN_POINT ( 'NONE',  ( 175.8776271403848739, -36.50981547336952104, 49.99999999999999289 ) ) ;
#8429 = LINE ( 'NONE', #2394, #1455 ) ;
#8430 = DIRECTION ( 'NONE',  ( -0.6692498792541753394, -0.7430374143461900838, 0.000000000000000000 ) ) ;
#8431 = LINE ( 'NONE', #6605, #18958 ) ;
#8432 = EDGE_LOOP ( 'NONE', ( #730, #1344, #5418, #113 ) ) ;
#8433 = CARTESIAN_POINT ( 'NONE',  ( 0.000000000000000000, 0.000000000000000000, 283.5832628385307999 ) ) ;
#8434 = CARTESIAN_POINT ( 'NONE',  ( -124.4044063703166785, -83.81803169341358739, -9.885272611403726373 ) ) ;
#8435 = CARTESIAN_POINT ( 'NONE',  ( 127.4413876050234933, 0.000000000000000000, 43.88498244535456649 ) ) ;
#8436 = LINE ( 'NONE', #14579, #17956 ) ;
#8437 = CYLINDRICAL_SURFACE ( 'NONE', #3322, 3.224098631618460331 ) ;
#8438 = CARTESIAN_POINT ( 'NONE',  ( 59.51724408343574879, -12.14957802882732452, 293.5832628385307999 ) ) ;
#8439 = CIRCLE ( 'NONE', #20192, 7.500000000000020428 ) ;
#8440 = ORIENTED_EDGE ( 'NONE', *, *, #15757, .F. ) ;
#8441 = VECTOR ( 'NONE', #19148, 1000.000000000000114 ) ;
#8442 = ORIENTED_EDGE ( 'NONE', *, *, #19307, .T. ) ;
#8443 = ORIENTED_EDGE ( 'NONE', *, *, #17420, .T. ) ;
#8444 = ORIENTED_EDGE ( 'NONE', *, *, #18599, .T. ) ;
#8445 = ORIENTED_EDGE ( 'NONE', *, *, #7011, .F. ) ;
#8446 = VECTOR ( 'NONE', #19666, 1000.000000000000000 ) ;
#8447 = ORIENTED_EDGE ( 'NONE', *, *, #19281, .T. ) ;
#8448 = AXIS2_PLACEMENT_3D ( 'NONE', #19129, #5116, #6249 ) ;
#8449 = CARTESIAN_POINT ( 'NONE',  ( -14.39940464655760799, -76.92888220842480962, 248.9926560891072143 ) ) ;
#8450 = VECTOR ( 'NONE', #7719, 1000.000000000000000 ) ;
#8451 = CARTESIAN_POINT ( 'NONE',  ( 67.36461649554532016, -39.84224160888924615, 132.4711112102474146 ) ) ;
#8452 = PLANE ( 'NONE',  #7773 ) ;
#8453 = ORIENTED_EDGE ( 'NONE', *, *, #14167, .T. ) ;
#8454 = DIRECTION ( 'NONE',  ( -0.8479630283625716469, 0.5300553768524345344, 0.000000000000000000 ) ) ;
#8455 = DIRECTION ( 'NONE',  ( -0.000000000000000000, -0.000000000000000000, 1.000000000000000000 ) ) ;
#8456 = ORIENTED_EDGE ( 'NONE', *, *, #11638, .T. ) ;
#8457 = CARTESIAN_POINT ( 'NONE',  ( 0.000000000000000000, 0.000000000000000000, 293.5832628385307999 ) ) ;
#8458 = CARTESIAN_POINT ( 'NONE',  ( 6.106329265062965028, -26.19668413589285194, 39.88498244535541204 ) ) ;
#8459 = CARTESIAN_POINT ( 'NONE',  ( 0.000000000000000000, 0.000000000000000000, 9.000000000000001776 ) ) ;
#8460 = CARTESIAN_POINT ( 'NONE',  ( 0.000000000000000000, 62.91752772691707207, 248.9926560891072143 ) ) ;
#8461 =( BOUNDED_SURFACE ( )  B_SPLINE_SURFACE ( 3, 2, ( 
 ( #8999, #15241, #1228 ),
 ( #1441, #16887, #2571 ),
 ( #12376, #7467, #16991 ),
 ( #15343, #1336, #13704 ),
 ( #13809, #10429, #2674 ),
 ( #8898, #4403, #5949 ),
 ( #2876, #20054, #15141 ),
 ( #18523, #1124, #7270 ) ),
 .UNSPECIFIED., .F., .F., .F. ) 
 B_SPLINE_SURFACE_WITH_KNOTS ( ( 4, 2, 2, 4 ),
 ( 3, 3 ),
 ( -0.01955877148976023494, -0.007974286041951373499, -0.002182043318046942345, 0.003610199405857488809 ),
 ( 0.7413449081104728222, 1.000000000000000000 ),
 .UNSPECIFIED. ) 
 GEOMETRIC_REPRESENTATION_ITEM ( )  RATIONAL_B_SPLINE_SURFACE ( (
 ( 0.9153618001336600862, 0.9429157744658526186, 1.000000000000000000),
 ( 0.9156768966432011769, 0.9431282912755682979, 1.000000000000000000),
 ( 0.9159077319687689567, 0.9432839781380815136, 1.000000000000000000),
 ( 0.9161393926374885588, 0.9434402216532019603, 1.000000000000000000),
 ( 0.9161974188647875605, 0.9434793574364683799, 1.000000000000000000),
 ( 0.9162751259529473558, 0.9435317669743971125, 1.000000000000000000),
 ( 0.9162946951553196939, 0.9435449654210028569, 1.000000000000000000),
 ( 0.9162945902535410969, 0.9435448946700086825, 1.000000000000000000) ) ) 
 REPRESENTATION_ITEM ( '' )  SURFACE ( )  );
#8462 = LINE ( 'NONE', #13248, #18565 ) ;
#8463 = DIRECTION ( 'NONE',  ( 1.000000000000000000, 0.000000000000000000, 0.000000000000000000 ) ) ;
#8464 = CARTESIAN_POINT ( 'NONE',  ( 126.5370453525553671, 80.55045718954892209, 60.00000000000000000 ) ) ;
#8465 = AXIS2_PLACEMENT_3D ( 'NONE', #5398, #14504, #6833 ) ;
#8466 = VECTOR ( 'NONE', #3455, 1000.000000000000227 ) ;
#8467 = ORIENTED_EDGE ( 'NONE', *, *, #19270, .T. ) ;
#8468 = EDGE_CURVE ( 'NONE', #9870, #10982, #4474, .T. ) ;
#8469 = CARTESIAN_POINT ( 'NONE',  ( 7.350000000000000533, -10.39230484541326582, 0.000000000000000000 ) ) ;
#8470 = ORIENTED_EDGE ( 'NONE', *, *, #18913, .F. ) ;
#8471 = VERTEX_POINT ( 'NONE', #2746 ) ;
#8472 = DIRECTION ( 'NONE',  ( 0.000000000000000000, 0.000000000000000000, 1.000000000000000000 ) ) ;
#8473 = ORIENTED_EDGE ( 'NONE', *, *, #16277, .F. ) ;
#8474 = FACE_OUTER_BOUND ( 'NONE', #12617, .T. ) ;
#8475 = EDGE_CURVE ( 'NONE', #15218, #3734, #5220, .T. ) ;
#8476 = CARTESIAN_POINT ( 'NONE',  ( -83.18633423686334538, -124.8217490215423879, 37.05209266191527462 ) ) ;
#8477 = EDGE_CURVE ( 'NONE', #9812, #17524, #9074, .T. ) ;
#8478 = FACE_BOUND ( 'NONE', #14442, .T. ) ;
#8479 = DIRECTION ( 'NONE',  ( -0.000000000000000000, -0.000000000000000000, -1.000000000000000000 ) ) ;
#8480 = VECTOR ( 'NONE', #4735, 1000.000000000000000 ) ;
#8481 = VECTOR ( 'NONE', #1590, 1000.000000000000000 ) ;
#8482 = EDGE_CURVE ( 'NONE', #19127, #19558, #9010, .T. ) ;
#8483 = ORIENTED_EDGE ( 'NONE', *, *, #8415, .F. ) ;
#8484 = DIRECTION ( 'NONE',  ( 0.000000000000000000, 0.000000000000000000, 1.000000000000000000 ) ) ;
#8485 = CARTESIAN_POINT ( 'NONE',  ( 53.40245231972179596, 28.94983032429848535, 293.5832628385307999 ) ) ;
#8486 = DIRECTION ( 'NONE',  ( 0.000000000000000000, 0.000000000000000000, 1.000000000000000000 ) ) ;
#8487 = CARTESIAN_POINT ( 'NONE',  ( 60.72073886220397299, -1.629865514042299512, 283.5832628385307999 ) ) ;
#8488 = ORIENTED_EDGE ( 'NONE', *, *, #13456, .T. ) ;
#8489 = CARTESIAN_POINT ( 'NONE',  ( 48.89172014028676472, 94.20918150411493741, 39.88498244535511361 ) ) ;
#8490 = DIRECTION ( 'NONE',  ( -0.000000000000000000, -0.000000000000000000, 1.000000000000000000 ) ) ;
#8491 = CARTESIAN_POINT ( 'NONE',  ( 100.7812500000000000, -111.0996833858562525, -10.00000000000000178 ) ) ;
#8492 = CARTESIAN_POINT ( 'NONE',  ( 0.000000000000000000, 164.0736214083062805, 39.99999999999999289 ) ) ;
#8493 = ORIENTED_EDGE ( 'NONE', *, *, #12992, .T. ) ;
#8494 = ADVANCED_FACE ( 'NONE', ( #17067 ), #3056, .T. ) ;
#8495 = CARTESIAN_POINT ( 'NONE',  ( 32.64570716507540737, -53.78543575132140830, 293.5832628385307999 ) ) ;
#8496 = CARTESIAN_POINT ( 'NONE',  ( 4.196299268919061021, 3.911853314815666671, 293.5832628385307999 ) ) ;
#8497 = EDGE_LOOP ( 'NONE', ( #13132, #20230, #7178, #7892 ) ) ;
#8498 = ORIENTED_EDGE ( 'NONE', *, *, #15802, .F. ) ;
#8499 = ITEM_DEFINED_TRANSFORMATION ( 'NONE', 'NONE', #16675,  #18639 ) ;
#8500 = CARTESIAN_POINT ( 'NONE',  ( 11.54085525628718401, 113.2974248684783163, 14.88498244535537296 ) ) ;
#8501 = B_SPLINE_CURVE_WITH_KNOTS ( 'NONE', 3,
 ( #15610, #7248, #15403, #18473, #10685, #13862, #1391, #15021 ),
 .UNSPECIFIED., .F., .F.,
 ( 4, 2, 2, 4 ),
 ( 0.01498083277331294441, 0.01629713195395221526, 0.01761343113459148957, 0.02024602949587003126 ),
 .UNSPECIFIED. ) ;
#8502 = ADVANCED_FACE ( 'NONE', ( #20228 ), #12447, .F. ) ;
#8503 = CARTESIAN_POINT ( 'NONE',  ( -85.53020504959707182, -140.9188050298390067, 39.99999999999999289 ) ) ;
#8504 = ORIENTED_EDGE ( 'NONE', *, *, #15223, .T. ) ;
#8505 = ADVANCED_FACE ( 'NONE', ( #3156 ), #15634, .T. ) ;
#8506 = CARTESIAN_POINT ( 'NONE',  ( 100.8144812491504325, -129.3825068912776999, 2.561523122930402074 ) ) ;
#8507 = CARTESIAN_POINT ( 'NONE',  ( -110.0000000000000142, 275.0000000000000000, 5.000000000000000888 ) ) ;
#8508 = CARTESIAN_POINT ( 'NONE',  ( -91.90390622750267369, -118.5498891763755864, -7.627268136224651940 ) ) ;
#8509 = ORIENTED_EDGE ( 'NONE', *, *, #4039, .T. ) ;
#8510 = ADVANCED_FACE ( 'NONE', ( #3558 ), #6728, .F. ) ;
#8511 = AXIS2_PLACEMENT_3D ( 'NONE', #89, #19122, #15541 ) ;
#8512 = PRODUCT_DEFINITION_FORMATION_WITH_SPECIFIED_SOURCE ( 'ANY', '', #513, .NOT_KNOWN. ) ;
#8513 = VECTOR ( 'NONE', #18216, 1000.000000000000114 ) ;
#8514 = DIRECTION ( 'NONE',  ( -0.7660444431189770143, 0.6427876096865404731, 5.346191897317644801E-15 ) ) ;
#8515 = CARTESIAN_POINT ( 'NONE',  ( 0.000000000000000000, 7.794228634059941818, 4.500000000000007994 ) ) ;
#8516 = CARTESIAN_POINT ( 'NONE',  ( -12.78021302872797449, 77.21438937758516374, 248.9926560891072143 ) ) ;
#8517 = LINE ( 'NONE', #10055, #11717 ) ;
#8518 = CARTESIAN_POINT ( 'NONE',  ( -110.0000000000000142, 285.0000000000000568, -94.99999999999997158 ) ) ;
#8519 = ORIENTED_EDGE ( 'NONE', *, *, #8391, .T. ) ;
#8520 = EDGE_CURVE ( 'NONE', #8371, #12416, #3100, .T. ) ;
#8521 = CARTESIAN_POINT ( 'NONE',  ( 100.7812500000000000, -111.0996833858562525, -10.00000000000000178 ) ) ;
#8522 = DIRECTION ( 'NONE',  ( 6.982962677686266711E-15, -0.000000000000000000, 1.000000000000000000 ) ) ;
#8523 = AXIS2_PLACEMENT_3D ( 'NONE', #14799, #3854, #10099 ) ;
#8524 = VECTOR ( 'NONE', #2350, 1000.000000000000000 ) ;
#8525 = ORIENTED_EDGE ( 'NONE', *, *, #14166, .T. ) ;
#8526 = ORIENTED_EDGE ( 'NONE', *, *, #15392, .T. ) ;
#8527 = EDGE_CURVE ( 'NONE', #16530, #1562, #2126, .T. ) ;
#8528 = EDGE_CURVE ( 'NONE', #7267, #22, #17177, .T. ) ;
#8529 = EDGE_CURVE ( 'NONE', #20114, #3604, #19111, .T. ) ;
#8530 = EDGE_CURVE ( 'NONE', #380, #12588, #15852, .T. ) ;
#8531 = CARTESIAN_POINT ( 'NONE',  ( 36.99387960884163107, -48.17797692984174063, 283.5832628385307999 ) ) ;
#8532 = LINE ( 'NONE', #6705, #3551 ) ;
#8533 = LINE ( 'NONE', #2304, #19586 ) ;
#8534 = ORIENTED_EDGE ( 'NONE', *, *, #10693, .F. ) ;
#8535 = CARTESIAN_POINT ( 'NONE',  ( 48.17959877923549072, 36.99514631729036296, 283.5832628385307999 ) ) ;
#8536 = DIRECTION ( 'NONE',  ( 0.000000000000000000, 0.000000000000000000, 1.000000000000000000 ) ) ;
#8537 = VECTOR ( 'NONE', #10763, 1000.000000000000000 ) ;
#8538 = LINE ( 'NONE', #14868, #6611 ) ;
#8539 = CARTESIAN_POINT ( 'NONE',  ( -135.1060089022256818, -65.16414933467417825, 10.00000000000000178 ) ) ;
#8540 = AXIS2_PLACEMENT_3D ( 'NONE', #7299, #8635, #19776 ) ;
#8541 = FACE_OUTER_BOUND ( 'NONE', #14074, .T. ) ;
#8542 = EDGE_LOOP ( 'NONE', ( #16915, #11105, #7777, #9835 ) ) ;
#8543 = VERTEX_POINT ( 'NONE', #1713 ) ;
#8544 = ORIENTED_EDGE ( 'NONE', *, *, #547, .F. ) ;
#8545 = ORIENTED_EDGE ( 'NONE', *, *, #17671, .T. ) ;
#8546 = FACE_OUTER_BOUND ( 'NONE', #4295, .T. ) ;
#8547 = VERTEX_POINT ( 'NONE', #3656 ) ;
#8548 = DIRECTION ( 'NONE',  ( 0.000000000000000000, 0.000000000000000000, -1.000000000000000000 ) ) ;
#8549 = CARTESIAN_POINT ( 'NONE',  ( 28.06680738835026290, -53.87178215532764369, 283.5832628385307999 ) ) ;
#8550 = CARTESIAN_POINT ( 'NONE',  ( 50.13752642112827829, 30.53958573130925558, 110.9660488491356887 ) ) ;
#8551 = ORIENTED_EDGE ( 'NONE', *, *, #13629, .T. ) ;
#8552 = CARTESIAN_POINT ( 'NONE',  ( -73.25972925305609351, 27.53920554013712874, 248.9926560891072143 ) ) ;
#8553 = DIRECTION ( 'NONE',  ( 0.3420201433256662704, 0.9396926207859092051, 0.000000000000000000 ) ) ;
#8554 = EDGE_CURVE ( 'NONE', #3346, #5032, #14197, .T. ) ;
#8555 = ORIENTED_EDGE ( 'NONE', *, *, #287, .T. ) ;
#8556 = DIRECTION ( 'NONE',  ( -1.000000000000000000, 0.000000000000000000, 0.000000000000000000 ) ) ;
#8557 = CYLINDRICAL_SURFACE ( 'NONE', #4456, 60.74260934110282051 ) ;
#8558 = CYLINDRICAL_SURFACE ( 'NONE', #4210, 60.74260934110282051 ) ;
#8559 = DIRECTION ( 'NONE',  ( -0.000000000000000000, -0.000000000000000000, -1.000000000000000000 ) ) ;
#8560 = LINE ( 'NONE', #14802, #2865 ) ;
#8561 = CARTESIAN_POINT ( 'NONE',  ( 27.90514497005392869, -110.4119590718113244, 39.88498244535525572 ) ) ;
#8562 = PLANE ( 'NONE',  #1861 ) ;
#8563 = VERTEX_POINT ( 'NONE', #15732 ) ;
#8564 = DIRECTION ( 'NONE',  ( -3.491481338843133355E-15, 1.000000000000000000, 0.000000000000000000 ) ) ;
#8565 = CIRCLE ( 'NONE', #4325, 3.224098631618461219 ) ;
#8566 = AXIS2_PLACEMENT_3D ( 'NONE', #8029, #3230, #11304 ) ;
#8567 = ORIENTED_EDGE ( 'NONE', *, *, #3471, .F. ) ;
#8568 = ORIENTED_EDGE ( 'NONE', *, *, #11419, .T. ) ;
#8569 = CARTESIAN_POINT ( 'NONE',  ( -110.0000000000000142, 275.0000000000000000, -75.00000000000000000 ) ) ;
#8570 = ORIENTED_EDGE ( 'NONE', *, *, #11030, .F. ) ;
#8571 = AXIS2_PLACEMENT_3D ( 'NONE', #6572, #14337, #19053 ) ;
#8572 = CIRCLE ( 'NONE', #20003, 62.91752772691707207 ) ;
#8573 = CARTESIAN_POINT ( 'NONE',  ( -110.0000000000000142, 265.0000000000000000, -67.49999999999997158 ) ) ;
#8574 = DIRECTION ( 'NONE',  ( 4.650550193362991910E-16, 1.000000000000000000, 0.000000000000000000 ) ) ;
#8575 = CARTESIAN_POINT ( 'NONE',  ( -5.693982670708905403, 0.7000608949449642626, 293.5832628385307999 ) ) ;
#8576 = CARTESIAN_POINT ( 'NONE',  ( -110.0000000000000000, 275.0000000000000000, 104.9999999999999858 ) ) ;
#8577 = EDGE_CURVE ( 'NONE', #912, #2426, #14576, .T. ) ;
#8578 = ORIENTED_EDGE ( 'NONE', *, *, #3968, .F. ) ;
#8579 = CARTESIAN_POINT ( 'NONE',  ( 14.39940464655707331, 76.92888220842492331, 112.0427633081292953 ) ) ;
#8581 = AXIS2_PLACEMENT_3D ( 'NONE', #18106, #915, #16576 ) ;
#8580 = LINE ( 'NONE', #804, #18577 ) ;
#8582 = CIRCLE ( 'NONE', #87, 150.0000000000000284 ) ;
#8583 = DIRECTION ( 'NONE',  ( 6.982962677686266711E-15, -0.000000000000000000, 1.000000000000000000 ) ) ;
#8584 = DIRECTION ( 'NONE',  ( 1.000000000000000000, 0.000000000000000000, 0.000000000000000000 ) ) ;
#8585 = ORIENTED_EDGE ( 'NONE', *, *, #16366, .T. ) ;
#8586 = LINE ( 'NONE', #5426, #16113 ) ;
#8587 = DIRECTION ( 'NONE',  ( 0.5000000000000009992, -0.8660254037844380415, -0.000000000000000000 ) ) ;
#8588 = AXIS2_PLACEMENT_3D ( 'NONE', #11444, #8269, #16260 ) ;
#8589 = CARTESIAN_POINT ( 'NONE',  ( 86.10242266703180292, -122.8274731153597799, -2.462352461605555654 ) ) ;
#8590 = CARTESIAN_POINT ( 'NONE',  ( 50.37374754117451658, -141.2886604036503115, 60.00000000000000000 ) ) ;
#8591 = VERTEX_POINT ( 'NONE', #6331 ) ;
#8592 = EDGE_CURVE ( 'NONE', #12327, #14347, #7948, .T. ) ;
#8593 = DIRECTION ( 'NONE',  ( 0.000000000000000000, 0.000000000000000000, 1.000000000000000000 ) ) ;
#8594 = LINE ( 'NONE', #11751, #6656 ) ;
#8595 = ORIENTED_EDGE ( 'NONE', *, *, #14270, .T. ) ;
#8596 = EDGE_LOOP ( 'NONE', ( #8986, #15082, #7016 ) ) ;
#8597 = VECTOR ( 'NONE', #10822, 1000.000000000000000 ) ;
#8598 = AXIS2_PLACEMENT_3D ( 'NONE', #1920, #1815, #17271 ) ;
#8599 = EDGE_LOOP ( 'NONE', ( #17999, #17197, #5335, #14175 ) ) ;
#8600 = PLANE ( 'NONE',  #14030 ) ;
#8601 = LINE ( 'NONE', #14932, #18186 ) ;
#8602 = EDGE_LOOP ( 'NONE', ( #14585, #15596, #11150 ) ) ;
#8603 = AXIS2_PLACEMENT_3D ( 'NONE', #13212, #11593, #17842 ) ;
#8604 = CARTESIAN_POINT ( 'NONE',  ( 100.6915138157988991, -129.5610470606159481, 2.673863972956103563 ) ) ;
#8605 = CARTESIAN_POINT ( 'NONE',  ( -96.12039245752636418, -116.0188909747188575, 9.827413591029802831 ) ) ;
#8606 = ORIENTED_EDGE ( 'NONE', *, *, #601, .T. ) ;
#8607 = EDGE_CURVE ( 'NONE', #19610, #16066, #12653, .T. ) ;
#8608 = CARTESIAN_POINT ( 'NONE',  ( -87.33261371895457614, -121.9603527571197787, -3.999215385619499408 ) ) ;
#8609 = DIRECTION ( 'NONE',  ( -0.000000000000000000, -1.000000000000000000, -0.000000000000000000 ) ) ;
#8610 = DIRECTION ( 'NONE',  ( 1.000000000000000000, 0.000000000000000000, 0.000000000000000000 ) ) ;
#8611 = AXIS2_PLACEMENT_3D ( 'NONE', #13253, #6841, #4057 ) ;
#8612 = CARTESIAN_POINT ( 'NONE',  ( -1.629865514042508456, -60.72073886220396588, 293.5832628385307999 ) ) ;
#8613 = FACE_OUTER_BOUND ( 'NONE', #3393, .T. ) ;
#8614 = EDGE_LOOP ( 'NONE', ( #6821, #3137, #4261, #3866 ) ) ;
#8615 = EDGE_CURVE ( 'NONE', #16737, #16978, #17200, .T. ) ;
#8616 = CARTESIAN_POINT ( 'NONE',  ( 120.7779226595531128, 102.2982297021113141, 49.99999999999999289 ) ) ;
#8617 = DIRECTION ( 'NONE',  ( -0.7660444431189862291, -0.6427876096865298150, 5.380491337840976593E-15 ) ) ;
#8618 = AXIS2_PLACEMENT_3D ( 'NONE', #9549, #18974, #232 ) ;
#8619 = EDGE_CURVE ( 'NONE', #15878, #573, #17813, .T. ) ;
#8620 = ORIENTED_EDGE ( 'NONE', *, *, #5742, .T. ) ;
#8621 = VECTOR ( 'NONE', #8964, 1000.000000000000114 ) ;
#8622 = EDGE_LOOP ( 'NONE', ( #7985, #14874, #11756, #13392 ) ) ;
#8623 = CARTESIAN_POINT ( 'NONE',  ( -176.5810126522742110, -187.6736222527391647, 8.827867842925929409 ) ) ;
#8624 = VERTEX_POINT ( 'NONE', #12599 ) ;
#8625 = CARTESIAN_POINT ( 'NONE',  ( 17.50000000000001066, 0.000000000000000000, 4.999999999999948486 ) ) ;
#8626 = ADVANCED_FACE ( 'NONE', ( #15690 ), #12705, .F. ) ;
#8627 = DIRECTION ( 'NONE',  ( -0.000000000000000000, -0.000000000000000000, 1.000000000000000000 ) ) ;
#8628 = DIRECTION ( 'NONE',  ( -0.000000000000000000, -0.000000000000000000, -1.000000000000000000 ) ) ;
#8629 = AXIS2_PLACEMENT_3D ( 'NONE', #11959, #8805, #3998 ) ;
#8630 = LINE ( 'NONE', #3924, #1967 ) ;
#8631 = DIRECTION ( 'NONE',  ( 1.000000000000000000, 0.000000000000000000, 0.000000000000000000 ) ) ;
#8632 = CARTESIAN_POINT ( 'NONE',  ( -129.1041139275565683, -76.37100075998222337, -7.395096211630200145 ) ) ;
#8633 = DIRECTION ( 'NONE',  ( 0.000000000000000000, 0.000000000000000000, -1.000000000000000000 ) ) ;
#8634 = VECTOR ( 'NONE', #3023, 1000.000000000000000 ) ;
#8635 = DIRECTION ( 'NONE',  ( 0.000000000000000000, 0.000000000000000000, 1.000000000000000000 ) ) ;
#8636 = DIRECTION ( 'NONE',  ( 0.9396926207859104263, 0.3420201433256630508, -6.584943678403439596E-15 ) ) ;
#8637 = ORIENTED_EDGE ( 'NONE', *, *, #10730, .T. ) ;
#8638 = EDGE_CURVE ( 'NONE', #2266, #13730, #3310, .T. ) ;
#8639 = EDGE_CURVE ( 'NONE', #12535, #3408, #18160, .T. ) ;
#8640 = PRODUCT_DEFINITION ( 'UNKNOWN', '', #12075, #13124 ) ;
#8641 = ORIENTED_EDGE ( 'NONE', *, *, #9875, .F. ) ;
#8642 = ORIENTED_EDGE ( 'NONE', *, *, #14102, .T. ) ;
#8643 = CIRCLE ( 'NONE', #11882, 3.224098631618455890 ) ;
#8644 = ORIENTED_EDGE ( 'NONE', *, *, #14588, .F. ) ;
#8645 = EDGE_LOOP ( 'NONE', ( #16583, #18903, #15023, #14554 ) ) ;
#8646 = DIRECTION ( 'NONE',  ( -3.129754055707530415E-16, 1.000000000000000000, -0.000000000000000000 ) ) ;
#8647 = CARTESIAN_POINT ( 'NONE',  ( -32.50000000000000000, 0.000000000000000000, -105.0000000000000142 ) ) ;
#8648 = CARTESIAN_POINT ( 'NONE',  ( 7.500000000000001776, 60.00000000000000000, -115.0000000000000000 ) ) ;
#8649 = FACE_OUTER_BOUND ( 'NONE', #15412, .T. ) ;
#8650 = ORIENTED_EDGE ( 'NONE', *, *, #8272, .F. ) ;
#8652 = CARTESIAN_POINT ( 'NONE',  ( -40.32479851956768613, 67.08601213326579682, 248.9926560891072143 ) ) ;
#8651 = CIRCLE ( 'NONE', #20087, 9.999999999999992895 ) ;
#8653 = DIRECTION ( 'NONE',  ( 0.000000000000000000, 1.000000000000000000, 0.000000000000000000 ) ) ;
#8654 = ORIENTED_EDGE ( 'NONE', *, *, #18633, .T. ) ;
#8655 = CARTESIAN_POINT ( 'NONE',  ( 41.48948842197119546, -47.29944656917770374, 293.5832628385307999 ) ) ;
#8656 = DIRECTION ( 'NONE',  ( 0.9271237148521548344, -0.3747554100459928317, 0.000000000000000000 ) ) ;
#8657 = CARTESIAN_POINT ( 'NONE',  ( -58.69016442926521648, -1.379293853801960124, 132.4711112102474146 ) ) ;
#8658 = AXIS2_PLACEMENT_3D ( 'NONE', #710, #19440, #13375 ) ;
#8659 = DIRECTION ( 'NONE',  ( 0.9848077530122097967, -0.1736481776669206722, 0.000000000000000000 ) ) ;
#8660 = EDGE_CURVE ( 'NONE', #18107, #6039, #14043, .T. ) ;
#8661 = FACE_OUTER_BOUND ( 'NONE', #2955, .T. ) ;
#8662 = DIRECTION ( 'NONE',  ( -0.000000000000000000, -0.000000000000000000, 1.000000000000000000 ) ) ;
#8663 = VERTEX_POINT ( 'NONE', #18659 ) ;
#8664 = DIRECTION ( 'NONE',  ( 0.000000000000000000, 0.000000000000000000, -1.000000000000000000 ) ) ;
#8665 = ORIENTED_EDGE ( 'NONE', *, *, #6398, .F. ) ;
#8666 = AXIS2_PLACEMENT_3D ( 'NONE', #1867, #13004, #6878 ) ;
#8667 = EDGE_CURVE ( 'NONE', #14077, #1203, #375, .T. ) ;
#8668 = VERTEX_POINT ( 'NONE', #9335 ) ;
#8669 = CARTESIAN_POINT ( 'NONE',  ( -110.0000000000000142, 285.0000000000000568, 5.000000000000000888 ) ) ;
#8670 = EDGE_LOOP ( 'NONE', ( #6831, #14018, #28, #8215 ) ) ;
#8671 = ORIENTED_EDGE ( 'NONE', *, *, #5936, .T. ) ;
#8672 = LINE ( 'NONE', #7149, #9434 ) ;
#8673 = DIRECTION ( 'NONE',  ( 1.000000000000000000, 0.000000000000000000, 0.000000000000000000 ) ) ;
#8674 = DIRECTION ( 'NONE',  ( 0.000000000000000000, 0.000000000000000000, -1.000000000000000000 ) ) ;
#8675 = FACE_OUTER_BOUND ( 'NONE', #17293, .T. ) ;
#8676 = AXIS2_PLACEMENT_3D ( 'NONE', #334, #11282, #9742 ) ;
#8677 = ORIENTED_EDGE ( 'NONE', *, *, #14413, .F. ) ;
#8678 = CARTESIAN_POINT ( 'NONE',  ( 14.85701326357409968, 22.71800723006099432, 14.88498244535534809 ) ) ;
#8679 = DIRECTION ( 'NONE',  ( 0.000000000000000000, 0.000000000000000000, 1.000000000000000000 ) ) ;
#8680 = VECTOR ( 'NONE', #10600, 1000.000000000000000 ) ;
#8681 = CARTESIAN_POINT ( 'NONE',  ( 0.000000000000000000, 60.00000000000000000, -100.0000000000000000 ) ) ;
#8682 = FACE_OUTER_BOUND ( 'NONE', #12219, .T. ) ;
#8683 = VERTEX_POINT ( 'NONE', #14354 ) ;
#8684 = CARTESIAN_POINT ( 'NONE',  ( 7.948937137877743808, -60.22232964560488000, 293.5832628385307999 ) ) ;
#8685 = CARTESIAN_POINT ( 'NONE',  ( 87.35350281426670449, -121.9411179691607003, -3.975120933794691336 ) ) ;
#8686 = PLANE ( 'NONE',  #3351 ) ;
#8687 = ORIENTED_EDGE ( 'NONE', *, *, #4686, .F. ) ;
#8688 = DIRECTION ( 'NONE',  ( -0.000000000000000000, -0.000000000000000000, 1.000000000000000000 ) ) ;
#8689 = DIRECTION ( 'NONE',  ( 0.000000000000000000, 0.000000000000000000, -1.000000000000000000 ) ) ;
#8690 = ORIENTED_EDGE ( 'NONE', *, *, #17948, .T. ) ;
#8691 = VECTOR ( 'NONE', #8484, 1000.000000000000000 ) ;
#8692 = ORIENTED_EDGE ( 'NONE', *, *, #1907, .F. ) ;
#8693 = AXIS2_PLACEMENT_3D ( 'NONE', #7940, #14191, #17372 ) ;
#8694 = ADVANCED_BREP_SHAPE_REPRESENTATION ( '', ( #1186, #18639 ), #14384 ) ;
#8695 = ORIENTED_EDGE ( 'NONE', *, *, #17533, .T. ) ;
#8696 = CARTESIAN_POINT ( 'NONE',  ( -60.83768308848345185, 49.24833719034248958, 132.4711112102474146 ) ) ;
#8697 = AXIS2_PLACEMENT_3D ( 'NONE', #13061, #7037, #982 ) ;
#8698 = DIRECTION ( 'NONE',  ( 1.000000000000000000, 0.000000000000000000, -0.000000000000000000 ) ) ;
#8699 = ORIENTED_EDGE ( 'NONE', *, *, #13672, .T. ) ;
#8700 = CARTESIAN_POINT ( 'NONE',  ( -175.4992877478424873, -40.00000000000000000, -115.0000000000000142 ) ) ;
#8701 = CARTESIAN_POINT ( 'NONE',  ( 6.106329265062790945, -26.19668413589285194, 14.88498244535541026 ) ) ;
#8702 = VECTOR ( 'NONE', #17280, 1000.000000000000114 ) ;
#8703 = CARTESIAN_POINT ( 'NONE',  ( -140.0000000000000568, -2.688074818803143362, 23.02775637731987501 ) ) ;
#8704 = DIRECTION ( 'NONE',  ( 1.000000000000000000, 0.000000000000000000, -0.000000000000000000 ) ) ;
#8705 = DIRECTION ( 'NONE',  ( -0.1736481776669172583, -0.9848077530122103518, 0.000000000000000000 ) ) ;
#8706 = CIRCLE ( 'NONE', #8395, 150.0000000000000284 ) ;
#8707 = CARTESIAN_POINT ( 'NONE',  ( 59.58067424803626722, -20.21777810286697985, 248.9926560891072143 ) ) ;
#8708 = CARTESIAN_POINT ( 'NONE',  ( -3.123743752083685266, 4.811834253408552087, 293.5832628385307999 ) ) ;
#8709 = DIRECTION ( 'NONE',  ( -1.000000000000000000, 0.000000000000000000, 0.000000000000000000 ) ) ;
#8710 = DIRECTION ( 'NONE',  ( -0.000000000000000000, -0.000000000000000000, 1.000000000000000000 ) ) ;
#8711 = ORIENTED_EDGE ( 'NONE', *, *, #1584, .F. ) ;
#8712 = CARTESIAN_POINT ( 'NONE',  ( 128.2779226595531270, 102.2982297021113141, 60.00000000000000000 ) ) ;
#8713 = LINE ( 'NONE', #11681, #16421 ) ;
#8714 = EDGE_CURVE ( 'NONE', #17576, #1080, #15216, .T. ) ;
#8715 = ORIENTED_EDGE ( 'NONE', *, *, #7993, .T. ) ;
#8716 = EDGE_LOOP ( 'NONE', ( #10375, #18183, #10740, #14418, #10651, #6539 ) ) ;
#8717 = CARTESIAN_POINT ( 'NONE',  ( 0.8220851292435327196, 58.69016442926522359, 248.9926560891072143 ) ) ;
#8718 = ORIENTED_EDGE ( 'NONE', *, *, #16159, .T. ) ;
#8719 = LINE ( 'NONE', #13311, #20035 ) ;
#8720 = DIRECTION ( 'NONE',  ( 0.000000000000000000, 0.000000000000000000, 1.000000000000000000 ) ) ;
#8721 = EDGE_CURVE ( 'NONE', #3127, #11536, #6382, .T. ) ;
#8722 = DIRECTION ( 'NONE',  ( -0.1390141521205912334, 0.9902903945359629034, 0.000000000000000000 ) ) ;
#8723 = ADVANCED_FACE ( 'NONE', ( #3505 ), #7802, .T. ) ;
#8724 = CARTESIAN_POINT ( 'NONE',  ( 5.111158570922254896, -2.605298826210304064, 293.5832628385307999 ) ) ;
#8725 = PLANE ( 'NONE',  #5899 ) ;
#8726 = ADVANCED_FACE ( 'NONE', ( #15990 ), #15263, .F. ) ;
#8727 = DIRECTION ( 'NONE',  ( -0.000000000000000000, -0.000000000000000000, 1.000000000000000000 ) ) ;
#8728 = CARTESIAN_POINT ( 'NONE',  ( -127.7402033587038375, -78.63140257242432085, -8.470234954248022419 ) ) ;
#8729 = FACE_OUTER_BOUND ( 'NONE', #13452, .T. ) ;
#8730 = DIRECTION ( 'NONE',  ( 0.5000000000000044409, 0.8660254037844360431, -4.304393070272782536E-15 ) ) ;
#8731 = CARTESIAN_POINT ( 'NONE',  ( 12.24586475280392506, -24.22555452564823497, 14.88498244535536585 ) ) ;
#8732 = DIRECTION ( 'NONE',  ( -0.7881095627315599650, -0.6155349844899714595, 0.000000000000000000 ) ) ;
#8733 = ORIENTED_EDGE ( 'NONE', *, *, #1685, .T. ) ;
#8734 = VECTOR ( 'NONE', #15260, 1000.000000000000114 ) ;
#8735 = EDGE_CURVE ( 'NONE', #17877, #11084, #10977, .T. ) ;
#8737 = ORIENTED_EDGE ( 'NONE', *, *, #11104, .F. ) ;
#8736 = CIRCLE ( 'NONE', #12673, 7.500000000000007105 ) ;
#8738 = EDGE_LOOP ( 'NONE', ( #12076, #13457 ) ) ;
#8739 = ORIENTED_EDGE ( 'NONE', *, *, #9357, .T. ) ;
#8740 = ORIENTED_EDGE ( 'NONE', *, *, #14167, .F. ) ;
#8741 = DIRECTION ( 'NONE',  ( -0.9902903945359624593, -0.1390141521205945918, 0.000000000000000000 ) ) ;
#8742 = CARTESIAN_POINT ( 'NONE',  ( -71.18887634719365565, -147.8252249328922687, 60.00000000000000000 ) ) ;
#8743 = VERTEX_POINT ( 'NONE', #12164 ) ;
#8744 = ADVANCED_FACE ( 'NONE', ( #18321 ), #13703, .F. ) ;
#8745 = CARTESIAN_POINT ( 'NONE',  ( 0.5584673446549131004, -9.967293815311094818, 0.7361406979141402740 ) ) ;
#8746 = CARTESIAN_POINT ( 'NONE',  ( 78.26059000578312919, -0.8220851292427129309, 248.9926560891072143 ) ) ;
#8747 = VECTOR ( 'NONE', #776, 1000.000000000000000 ) ;
#8748 = EDGE_CURVE ( 'NONE', #17524, #9946, #8801, .T. ) ;
#8749 = ORIENTED_EDGE ( 'NONE', *, *, #17619, .F. ) ;
#8750 = DIRECTION ( 'NONE',  ( 1.000000000000000000, -0.000000000000000000, -0.000000000000000000 ) ) ;
#8751 = VECTOR ( 'NONE', #1753, 1000.000000000000000 ) ;
#8752 = LINE ( 'NONE', #7318, #10011 ) ;
#8753 = FACE_OUTER_BOUND ( 'NONE', #14535, .T. ) ;
#8754 = CARTESIAN_POINT ( 'NONE',  ( -60.83768308848343764, 49.24833719034248958, 110.7293897666001214 ) ) ;
#8755 = CARTESIAN_POINT ( 'NONE',  ( 124.4044063703119321, -83.81803169342077808, 49.88527261140372815 ) ) ;
#8756 = DIRECTION ( 'NONE',  ( -0.6155349844899689060, 0.7881095627315620744, 0.000000000000000000 ) ) ;
#8757 = ORIENTED_EDGE ( 'NONE', *, *, #18025, .T. ) ;
#8758 = EDGE_CURVE ( 'NONE', #7379, #18614, #15043, .T. ) ;
#8759 = CARTESIAN_POINT ( 'NONE',  ( -110.0000000000000142, 265.0000000000000000, -75.00000000000000000 ) ) ;
#8760 = AXIS2_PLACEMENT_3D ( 'NONE', #1946, #8177, #19131 ) ;
#8761 = ORIENTED_EDGE ( 'NONE', *, *, #11040, .F. ) ;
#8762 = AXIS2_PLACEMENT_3D ( 'NONE', #1639, #1729, #14005 ) ;
#8763 = VECTOR ( 'NONE', #13572, 1000.000000000000227 ) ;
#8764 = ORIENTED_EDGE ( 'NONE', *, *, #9766, .F. ) ;
#8765 = FACE_OUTER_BOUND ( 'NONE', #16186, .T. ) ;
#8766 = VECTOR ( 'NONE', #6407, 1000.000000000000000 ) ;
#8767 = ORIENTED_EDGE ( 'NONE', *, *, #12607, .F. ) ;
#8768 = EDGE_LOOP ( 'NONE', ( #11204, #16683, #17809 ) ) ;
#8769 = DIRECTION ( 'NONE',  ( -0.000000000000000000, -0.000000000000000000, 1.000000000000000000 ) ) ;
#8770 = CARTESIAN_POINT ( 'NONE',  ( -100.7812499999999716, -111.0996833858562809, 49.99999999999999289 ) ) ;
#8771 = EDGE_CURVE ( 'NONE', #10487, #6802, #7365, .T. ) ;
#8772 = DIRECTION ( 'NONE',  ( 1.000000000000000000, 0.000000000000000000, 0.000000000000000000 ) ) ;
#8773 = FACE_OUTER_BOUND ( 'NONE', #5212, .T. ) ;
#8774 = EDGE_CURVE ( 'NONE', #5714, #3545, #7180, .T. ) ;
#8775 = EDGE_LOOP ( 'NONE', ( #8924, #1557, #9935, #1162 ) ) ;
#8776 = LINE ( 'NONE', #11929, #8051 ) ;
#8777 = LINE ( 'NONE', #4276, #8127 ) ;
#8778 = VECTOR ( 'NONE', #11963, 999.9999999999998863 ) ;
#8779 = AXIS2_PLACEMENT_3D ( 'NONE', #4563, #17048, #4670 ) ;
#8780 = VECTOR ( 'NONE', #10916, 1000.000000000000114 ) ;
#8781 = EDGE_CURVE ( 'NONE', #4188, #19638, #13807, .T. ) ;
#8782 = DIRECTION ( 'NONE',  ( 1.000000000000000000, 0.000000000000000000, -0.000000000000000000 ) ) ;
#8783 = FACE_OUTER_BOUND ( 'NONE', #13717, .T. ) ;
#8784 = AXIS2_PLACEMENT_3D ( 'NONE', #17849, #3826, #6906 ) ;
#8785 = EDGE_LOOP ( 'NONE', ( #9009, #6044, #18108, #6614 ) ) ;
#8786 = CARTESIAN_POINT ( 'NONE',  ( -109.9999999999983515, 285.0000000000000568, 85.00000000000001421 ) ) ;
#8787 = CARTESIAN_POINT ( 'NONE',  ( 83.18633423686338801, -124.8217490215423737, 2.947907338084742701 ) ) ;
#8788 = CARTESIAN_POINT ( 'NONE',  ( -50.41613078340781584, 30.05702882063080494, 110.9660488491356887 ) ) ;
#8789 = ORIENTED_EDGE ( 'NONE', *, *, #6647, .T. ) ;
#8790 = DIRECTION ( 'NONE',  ( 0.9993852124581887875, -0.03505990758545544927, 0.000000000000000000 ) ) ;
#8791 = DIRECTION ( 'NONE',  ( -0.000000000000000000, -0.000000000000000000, 1.000000000000000000 ) ) ;
#8792 = ORIENTED_EDGE ( 'NONE', *, *, #6227, .F. ) ;
#8793 = EDGE_LOOP ( 'NONE', ( #12051, #4289, #9782, #4782 ) ) ;
#8794 = LINE ( 'NONE', #4189, #13997 ) ;
#8795 = AXIS2_PLACEMENT_3D ( 'NONE', #6515, #12734, #9224 ) ;
#8796 = CIRCLE ( 'NONE', #950, 60.74260934110282051 ) ;
#8797 = DIRECTION ( 'NONE',  ( -0.000000000000000000, -0.000000000000000000, 1.000000000000000000 ) ) ;
#8798 = CARTESIAN_POINT ( 'NONE',  ( -167.4599531637108782, -36.50981547337168109, 60.00000000000000000 ) ) ;
#8799 = VERTEX_POINT ( 'NONE', #19744 ) ;
#8800 = CARTESIAN_POINT ( 'NONE',  ( 92.40373333587093896, -118.1608478542247553, -7.903026561454264076 ) ) ;
#8801 = LINE ( 'NONE', #13596, #17152 ) ;
#8802 =( REPRESENTATION_RELATIONSHIP ('NONE','NONE', #17382, #7558 ) REPRESENTATION_RELATIONSHIP_WITH_TRANSFORMATION ( #14444 )SHAPE_REPRESENTATION_RELATIONSHIP( ) );
#8803 = CARTESIAN_POINT ( 'NONE',  ( 40.28046525994349736, 45.46865632508086463, 293.5832628385307999 ) ) ;
#8804 = CARTESIAN_POINT ( 'NONE',  ( 77.31114765718494652, -12.23146955673620084, 248.9926560891072143 ) ) ;
#8805 = DIRECTION ( 'NONE',  ( -6.982962677686266711E-15, 0.000000000000000000, -1.000000000000000000 ) ) ;
#8806 = CARTESIAN_POINT ( 'NONE',  ( -25.47323767126238181, -97.89424917625660783, 14.88498244535562876 ) ) ;
#8807 = CARTESIAN_POINT ( 'NONE',  ( -134.8030718230775449, -47.09494809331346232, 49.99999999999999289 ) ) ;
#8808 = CARTESIAN_POINT ( 'NONE',  ( 0.000000000000000000, 0.000000000000000000, 248.9926560891072143 ) ) ;
#8809 = AXIS2_PLACEMENT_3D ( 'NONE', #5463, #13218, #19480 ) ;
#8810 = ORIENTED_EDGE ( 'NONE', *, *, #13356, .T. ) ;
#8811 = DIRECTION ( 'NONE',  ( -0.9902903945359630145, -0.1390141521205912334, 0.000000000000000000 ) ) ;
#8812 = DIRECTION ( 'NONE',  ( 6.982962677686266711E-15, 0.000000000000000000, 1.000000000000000000 ) ) ;
#8813 = ORIENTED_EDGE ( 'NONE', *, *, #13431, .T. ) ;
#8814 = ORIENTED_EDGE ( 'NONE', *, *, #15257, .F. ) ;
#8815 = VERTEX_POINT ( 'NONE', #19647 ) ;
#8816 = VECTOR ( 'NONE', #18717, 1000.000000000000000 ) ;
#8817 = DIRECTION ( 'NONE',  ( -0.000000000000000000, -0.000000000000000000, 1.000000000000000000 ) ) ;
#8818 = AXIS2_PLACEMENT_3D ( 'NONE', #14034, #9537, #13926 ) ;
#8819 = VERTEX_POINT ( 'NONE', #15140 ) ;
#8820 = AXIS2_PLACEMENT_3D ( 'NONE', #5157, #6489, #9548 ) ;
#8821 = CARTESIAN_POINT ( 'NONE',  ( 133.8357118474723677, -78.97256401901070433, 2.952839103891145900 ) ) ;
#8822 = CARTESIAN_POINT ( 'NONE',  ( 79.75827554147308263, 0.000000000000000000, 293.5832628385307999 ) ) ;
#8823 = DIRECTION ( 'NONE',  ( -0.000000000000000000, -0.000000000000000000, 1.000000000000000000 ) ) ;
#8824 = CARTESIAN_POINT ( 'NONE',  ( -98.08520584366951311, -113.5061255252650483, 38.12154030620245493 ) ) ;
#8825 = PLANE ( 'NONE',  #3789 ) ;
#8826 = CARTESIAN_POINT ( 'NONE',  ( -78.26059000578311498, 0.8220851292432594937, 112.7772637782949516 ) ) ;
#8827 = ADVANCED_FACE ( 'NONE', ( #5637 ), #2470, .F. ) ;
#8828 = ORIENTED_EDGE ( 'NONE', *, *, #17763, .F. ) ;
#8829 = FACE_OUTER_BOUND ( 'NONE', #7013, .T. ) ;
#8830 = DIRECTION ( 'NONE',  ( 0.000000000000000000, 0.000000000000000000, 1.000000000000000000 ) ) ;
#8831 = DIRECTION ( 'NONE',  ( -1.000000000000000000, 0.000000000000000000, 0.000000000000000000 ) ) ;
#8832 = LINE ( 'NONE', #19777, #4479 ) ;
#8833 = DIRECTION ( 'NONE',  ( -0.7430374143461878633, 0.6692498792541777819, 0.000000000000000000 ) ) ;
#8834 = VERTEX_POINT ( 'NONE', #8701 ) ;
#8835 = ORIENTED_EDGE ( 'NONE', *, *, #8246, .T. ) ;
#8836 = EDGE_CURVE ( 'NONE', #11005, #16596, #8996, .T. ) ;
#8837 = ORIENTED_EDGE ( 'NONE', *, *, #5262, .T. ) ;
#8838 = VERTEX_POINT ( 'NONE', #10428 ) ;
#8839 = EDGE_CURVE ( 'NONE', #1401, #19110, #12564, .T. ) ;
#8840 = ORIENTED_EDGE ( 'NONE', *, *, #1979, .F. ) ;
#8841 = DIRECTION ( 'NONE',  ( -1.000000000000000000, 1.224646799147352961E-16, 0.000000000000000000 ) ) ;
#8842 = CIRCLE ( 'NONE', #11131, 62.91752772691707207 ) ;
#8843 = PLANE ( 'NONE',  #19426 ) ;
#8844 = LINE ( 'NONE', #12106, #10701 ) ;
#8845 = ORIENTED_EDGE ( 'NONE', *, *, #4258, .F. ) ;
#8846 = AXIS2_PLACEMENT_3D ( 'NONE', #4127, #18147, #10358 ) ;
#8847 = DIRECTION ( 'NONE',  ( -0.9781142164131917394, 0.2080686897406911207, 0.000000000000000000 ) ) ;
#8848 = CARTESIAN_POINT ( 'NONE',  ( 62.95000000000000284, 0.000000000000000000, 0.000000000000000000 ) ) ;
#8849 = ADVANCED_FACE ( 'NONE', ( #5948, #18425 ), #7463, .F. ) ;
#8850 = EDGE_LOOP ( 'NONE', ( #7867, #3239, #777, #18676 ) ) ;
#8851 = DIRECTION ( 'NONE',  ( -0.1736481776669374644, 0.9848077530122066880, -0.000000000000000000 ) ) ;
#8852 = CARTESIAN_POINT ( 'NONE',  ( -17.50000000000001776, 2.143131898507868643E-15, 39.88498244535557546 ) ) ;
#8853 = CARTESIAN_POINT ( 'NONE',  ( -134.7188131032333445, -72.93593548660989256, 10.00000000000000178 ) ) ;
#8854 = CARTESIAN_POINT ( 'NONE',  ( 107.5000000000000284, -118.5063289449133492, 50.00000000000000000 ) ) ;
#8855 = CARTESIAN_POINT ( 'NONE',  ( 127.3324793557656136, -79.33838548636531129, 40.86166200754897204 ) ) ;
#8856 = DIRECTION ( 'NONE',  ( 1.000000000000000000, 0.000000000000000000, 0.000000000000000000 ) ) ;
#8857 = ORIENTED_EDGE ( 'NONE', *, *, #19418, .T. ) ;
#8858 = EDGE_CURVE ( 'NONE', #11398, #15547, #10627, .T. ) ;
#8859 = CARTESIAN_POINT ( 'NONE',  ( -36.71940246244744799, 108.6254278180370250, 14.88498244535570869 ) ) ;
#8860 = ORIENTED_EDGE ( 'NONE', *, *, #9863, .F. ) ;
#8861 = EDGE_CURVE ( 'NONE', #7743, #14775, #18522, .T. ) ;
#8862 = ORIENTED_EDGE ( 'NONE', *, *, #11250, .T. ) ;
#8863 = EDGE_CURVE ( 'NONE', #13278, #9985, #7670, .T. ) ;
#8864 = CARTESIAN_POINT ( 'NONE',  ( -110.0000000000000000, 265.0000000000000000, 104.9999999999999858 ) ) ;
#8865 = VERTEX_POINT ( 'NONE', #15450 ) ;
#8866 = ORIENTED_EDGE ( 'NONE', *, *, #18134, .T. ) ;
#8867 = CARTESIAN_POINT ( 'NONE',  ( 0.000000000000000000, 0.000000000000000000, 283.5832628385307999 ) ) ;
#8868 = DIRECTION ( 'NONE',  ( -6.982962677686266711E-15, 0.000000000000000000, -1.000000000000000000 ) ) ;
#8869 = DIRECTION ( 'NONE',  ( -0.000000000000000000, -0.000000000000000000, 1.000000000000000000 ) ) ;
#8870 = CARTESIAN_POINT ( 'NONE',  ( -32.62092819947992695, -51.24245927909985454, 293.5832628385307999 ) ) ;
#8871 = ORIENTED_EDGE ( 'NONE', *, *, #14113, .T. ) ;
#8872 = EDGE_CURVE ( 'NONE', #10010, #13503, #18837, .T. ) ;
#8873 = CARTESIAN_POINT ( 'NONE',  ( -132.4400928985788823, -70.43137869103949811, 42.82464599639617120 ) ) ;
#8874 = DIRECTION ( 'NONE',  ( -0.000000000000000000, -0.000000000000000000, 1.000000000000000000 ) ) ;
#8875 = DIRECTION ( 'NONE',  ( -0.9511061040868794558, -0.3088643371590157338, 0.000000000000000000 ) ) ;
#8876 = ORIENTED_EDGE ( 'NONE', *, *, #4494, .F. ) ;
#8877 = AXIS2_PLACEMENT_3D ( 'NONE', #4748, #3511, #8106 ) ;
#8878 = DIRECTION ( 'NONE',  ( -0.8660254037844344888, -0.5000000000000069944, 0.000000000000000000 ) ) ;
#8879 = LINE ( 'NONE', #1205, #6226 ) ;
#8880 = CYLINDRICAL_SURFACE ( 'NONE', #16105, 7.500000000000001776 ) ;
#8881 = ORIENTED_EDGE ( 'NONE', *, *, #10331, .T. ) ;
#8882 = DIRECTION ( 'NONE',  ( 1.000000000000000000, 0.000000000000000000, 0.000000000000000000 ) ) ;
#8883 = DIRECTION ( 'NONE',  ( -0.000000000000000000, -0.000000000000000000, 1.000000000000000000 ) ) ;
#8884 = EDGE_LOOP ( 'NONE', ( #3597, #3608, #19886, #10057 ) ) ;
#8885 = EDGE_CURVE ( 'NONE', #7238, #2129, #15662, .T. ) ;
#8886 = EDGE_CURVE ( 'NONE', #15222, #6324, #12678, .T. ) ;
#8887 = ORIENTED_EDGE ( 'NONE', *, *, #2310, .F. ) ;
#8888 = EDGE_CURVE ( 'NONE', #1501, #10728, #306, .T. ) ;
#8889 = ADVANCED_FACE ( 'NONE', ( #1439 ), #6257, .T. ) ;
#8890 = CARTESIAN_POINT ( 'NONE',  ( -97.60910239587758497, -133.8115172545150529, 31.48501029038536814 ) ) ;
#8891 = VERTEX_POINT ( 'NONE', #4822 ) ;
#8892 = DIRECTION ( 'NONE',  ( 6.982962677686266711E-15, -0.000000000000000000, 1.000000000000000000 ) ) ;
#8893 = DIRECTION ( 'NONE',  ( -0.000000000000000000, -0.000000000000000000, 1.000000000000000000 ) ) ;
#8894 = AXIS2_PLACEMENT_3D ( 'NONE', #19421, #2705, #18253 ) ;
#8895 = ORIENTED_EDGE ( 'NONE', *, *, #19258, .T. ) ;
#8896 = CARTESIAN_POINT ( 'NONE',  ( -49.67518383744793908, 60.47951622432801599, 248.9926560891072143 ) ) ;
#8897 = DIRECTION ( 'NONE',  ( -0.000000000000000000, -0.000000000000000000, 1.000000000000000000 ) ) ;
#8898 = CARTESIAN_POINT ( 'NONE',  ( -141.6220008579448972, -18.66460740341266700, -11.97000856754251785 ) ) ;
#8899 = PLANE ( 'NONE',  #6029 ) ;
#8900 = CARTESIAN_POINT ( 'NONE',  ( -163.5019688434124419, -20.99123081650240863, 39.99999999999999289 ) ) ;
#8901 = PLANE ( 'NONE',  #17546 ) ;
#8902 = DIRECTION ( 'NONE',  ( -0.000000000000000000, -0.000000000000000000, 1.000000000000000000 ) ) ;
#8903 = CARTESIAN_POINT ( 'NONE',  ( 163.5019688434126977, -20.99123081650019529, 49.99999999999999289 ) ) ;
#8904 = ORIENTED_EDGE ( 'NONE', *, *, #8888, .T. ) ;
#8905 = DIRECTION ( 'NONE',  ( -0.000000000000000000, -1.000000000000000000, -0.000000000000000000 ) ) ;
#8906 = CARTESIAN_POINT ( 'NONE',  ( 81.66698895276879000, 79.37254397626031732, 14.88498244535488269 ) ) ;
#8907 = CIRCLE ( 'NONE', #16433, 6.000000000000001776 ) ;
#8908 = AXIS2_PLACEMENT_3D ( 'NONE', #5966, #9229, #12186 ) ;
#8909 = ADVANCED_FACE ( 'NONE', ( #15862 ), #17199, .F. ) ;
#8910 = VERTEX_POINT ( 'NONE', #7872 ) ;
#8911 = ORIENTED_EDGE ( 'NONE', *, *, #13431, .F. ) ;
#8912 = AXIS2_PLACEMENT_3D ( 'NONE', #11634, #17597, #3674 ) ;
#8913 = ORIENTED_EDGE ( 'NONE', *, *, #16912, .T. ) ;
#8914 = EDGE_CURVE ( 'NONE', #11201, #14920, #16217, .T. ) ;
#8915 = DIRECTION ( 'NONE',  ( 0.000000000000000000, 0.000000000000000000, -1.000000000000000000 ) ) ;
#8916 = CIRCLE ( 'NONE', #19081, 99.99999999999997158 ) ;
#8917 = ORIENTED_EDGE ( 'NONE', *, *, #8017, .F. ) ;
#8918 = CARTESIAN_POINT ( 'NONE',  ( 133.1920331248151115, -82.53376026279583755, 1.486861419600814305 ) ) ;
#8919 = CARTESIAN_POINT ( 'NONE',  ( -32.64570716507503079, 53.78543575132162857, 132.4711112102474146 ) ) ;
#8920 = CIRCLE ( 'NONE', #4020, 17.50000000000001066 ) ;
#8921 = CARTESIAN_POINT ( 'NONE',  ( 7.350000000000001421, 0.000000000000000000, 9.000000000000000000 ) ) ;
#8922 = LINE ( 'NONE', #19770, #1163 ) ;
#8923 = CARTESIAN_POINT ( 'NONE',  ( 0.000000000000000000, 0.000000000000000000, 283.5832628385307999 ) ) ;
#8924 = ORIENTED_EDGE ( 'NONE', *, *, #13759, .F. ) ;
#8925 = DIRECTION ( 'NONE',  ( -0.9749279121818261729, 0.2225209339563031519, 0.000000000000000000 ) ) ;
#8926 = CARTESIAN_POINT ( 'NONE',  ( -133.8517991834421821, -78.87665408946898538, 3.000515938330789112 ) ) ;
#8927 = CARTESIAN_POINT ( 'NONE',  ( 133.5298479455745735, -80.72596075551817307, 2.158131001320439335 ) ) ;
#8928 = VECTOR ( 'NONE', #2097, 1000.000000000000000 ) ;
#8929 = DIRECTION ( 'NONE',  ( 0.000000000000000000, 0.000000000000000000, -1.000000000000000000 ) ) ;
#8930 = CARTESIAN_POINT ( 'NONE',  ( 133.2435246741110006, -68.89240257401093004, 30.00000000000000000 ) ) ;
#8931 = LINE ( 'NONE', #957, #12909 ) ;
#8932 = EDGE_LOOP ( 'NONE', ( #5380, #44 ) ) ;
#8933 = DIRECTION ( 'NONE',  ( -0.000000000000000000, -0.000000000000000000, 1.000000000000000000 ) ) ;
#8934 = AXIS2_PLACEMENT_3D ( 'NONE', #5511, #11733, #3965 ) ;
#8935 = ORIENTED_EDGE ( 'NONE', *, *, #498, .F. ) ;
#8936 = VERTEX_POINT ( 'NONE', #20153 ) ;
#8937 = EDGE_LOOP ( 'NONE', ( #7377, #4508, #14235, #13959 ) ) ;
#8938 = ORIENTED_EDGE ( 'NONE', *, *, #15342, .T. ) ;
#8939 = AXIS2_PLACEMENT_3D ( 'NONE', #10431, #15143, #2286 ) ;
#8940 = LINE ( 'NONE', #18263, #6032 ) ;
#8941 = AXIS2_PLACEMENT_3D ( 'NONE', #5269, #5460, #14467 ) ;
#8942 = CARTESIAN_POINT ( 'NONE',  ( 0.2993243175132189737, -5.729042578294415655, 283.5832628385307999 ) ) ;
#8943 = ORIENTED_EDGE ( 'NONE', *, *, #631, .T. ) ;
#8944 = FACE_OUTER_BOUND ( 'NONE', #16537, .T. ) ;
#8945 = CARTESIAN_POINT ( 'NONE',  ( 0.000000000000000000, 0.000000000000000000, 0.000000000000000000 ) ) ;
#8946 = EDGE_LOOP ( 'NONE', ( #18062, #1640 ) ) ;
#8947 = CARTESIAN_POINT ( 'NONE',  ( 73.25972925305629246, -27.53920554013664912, 132.4711112102474146 ) ) ;
#8948 = FACE_OUTER_BOUND ( 'NONE', #13774, .T. ) ;
#8949 = DIRECTION ( 'NONE',  ( 0.000000000000000000, 0.000000000000000000, 1.000000000000000000 ) ) ;
#8950 = CARTESIAN_POINT ( 'NONE',  ( 106.6880305650188347, 105.4403344747995988, 60.00000000000000000 ) ) ;
#8951 = LINE ( 'NONE', #7525, #6485 ) ;
#8952 = CIRCLE ( 'NONE', #1452, 62.91752772691707207 ) ;
#8953 = DIRECTION ( 'NONE',  ( -0.000000000000000000, -0.000000000000000000, -1.000000000000000000 ) ) ;
#8954 = ORIENTED_EDGE ( 'NONE', *, *, #10331, .F. ) ;
#8955 = LINE ( 'NONE', #4463, #8357 ) ;
#8956 = ORIENTED_EDGE ( 'NONE', *, *, #18540, .F. ) ;
#8957 = ORIENTED_EDGE ( 'NONE', *, *, #14652, .T. ) ;
#8958 = ADVANCED_FACE ( 'NONE', ( #15555 ), #17304, .T. ) ;
#8959 = CARTESIAN_POINT ( 'NONE',  ( -109.5721339228237667, 31.03941509555038181, 14.88498244535621851 ) ) ;
#8960 = EDGE_LOOP ( 'NONE', ( #16798, #1381, #3797, #19489 ) ) ;
#8961 = ORIENTED_EDGE ( 'NONE', *, *, #17533, .F. ) ;
#8962 = VECTOR ( 'NONE', #16883, 1000.000000000000000 ) ;
#8963 = DIRECTION ( 'NONE',  ( 0.000000000000000000, 0.000000000000000000, -1.000000000000000000 ) ) ;
#8964 = DIRECTION ( 'NONE',  ( -0.3420201433256757073, 0.9396926207859057634, -0.000000000000000000 ) ) ;
#8965 = CYLINDRICAL_SURFACE ( 'NONE', #11362, 7.500000000000006217 ) ;
#8966 = ORIENTED_EDGE ( 'NONE', *, *, #17374, .F. ) ;
#8967 = AXIS2_PLACEMENT_3D ( 'NONE', #11126, #12764, #1718 ) ;
#8968 = CARTESIAN_POINT ( 'NONE',  ( 0.000000000000000000, 7.794228634059940930, -4.500000000000011546 ) ) ;
#8969 = CARTESIAN_POINT ( 'NONE',  ( -23.19741967113669290, 4.658826548058537576, 14.88498244535561277 ) ) ;
#8970 = ORIENTED_EDGE ( 'NONE', *, *, #1509, .T. ) ;
#8971 = EDGE_CURVE ( 'NONE', #2011, #18719, #4417, .T. ) ;
#8972 = DIRECTION ( 'NONE',  ( 1.000000000000000000, 0.000000000000000000, -0.000000000000000000 ) ) ;
#8973 = LINE ( 'NONE', #18499, #19561 ) ;
#8974 = EDGE_CURVE ( 'NONE', #4841, #10024, #1541, .T. ) ;
#8975 = ADVANCED_FACE ( 'NONE', ( #3079 ), #3181, .F. ) ;
#8976 = CARTESIAN_POINT ( 'NONE',  ( -53.40063514825077107, -28.94886449118923011, 283.5832628385307999 ) ) ;
#8977 = ORIENTED_EDGE ( 'NONE', *, *, #14138, .T. ) ;
#8978 = CARTESIAN_POINT ( 'NONE',  ( -40.27908801169994035, -45.46712722958821473, 293.5832628385307999 ) ) ;
#8979 = CARTESIAN_POINT ( 'NONE',  ( -134.7188131032333160, -72.93593548660990677, 30.49674468329109445 ) ) ;
#8980 = AXIS2_PLACEMENT_3D ( 'NONE', #11450, #12978, #2152 ) ;
#8981 = CARTESIAN_POINT ( 'NONE',  ( 0.000000000000000000, 0.000000000000000000, 132.4711112102474146 ) ) ;
#8982 = ORIENTED_EDGE ( 'NONE', *, *, #2283, .F. ) ;
#8983 = CARTESIAN_POINT ( 'NONE',  ( -71.18887634719365565, -147.8252249328922687, 49.99999999999999289 ) ) ;
#8984 = DIRECTION ( 'NONE',  ( 0.000000000000000000, 0.000000000000000000, -1.000000000000000000 ) ) ;
#8985 = VERTEX_POINT ( 'NONE', #12469 ) ;
#8986 = ORIENTED_EDGE ( 'NONE', *, *, #16984, .T. ) ;
#8987 = ADVANCED_FACE ( 'NONE', ( #14115 ), #12783, .F. ) ;
#8988 = CARTESIAN_POINT ( 'NONE',  ( -97.91442649640831064, -133.4097810206876034, 32.94424152684068474 ) ) ;
#8989 = ORIENTED_EDGE ( 'NONE', *, *, #12218, .F. ) ;
#8990 = AXIS2_PLACEMENT_3D ( 'NONE', #4159, #13662, #15304 ) ;
#8991 = DIRECTION ( 'NONE',  ( 0.9009688679024154823, 0.4338837391175657809, 0.000000000000000000 ) ) ;
#8992 = DIRECTION ( 'NONE',  ( 0.000000000000000000, 0.000000000000000000, 1.000000000000000000 ) ) ;
#8993 = ORIENTED_EDGE ( 'NONE', *, *, #13003, .F. ) ;
#8994 = AXIS2_PLACEMENT_3D ( 'NONE', #13491, #10326, #1022 ) ;
#8995 = CARTESIAN_POINT ( 'NONE',  ( -4.196299268919065462, -3.911853314815649796, 283.5832628385307999 ) ) ;
#8996 = LINE ( 'NONE', #4196, #8962 ) ;
#8997 = EDGE_CURVE ( 'NONE', #19717, #98, #14222, .T. ) ;
#8998 = EDGE_CURVE ( 'NONE', #9304, #10138, #14855, .T. ) ;
#8999 = CARTESIAN_POINT ( 'NONE',  ( -139.5603828663319916, -18.86179323242330952, -21.49533993996032066 ) ) ;
#9000 = DIRECTION ( 'NONE',  ( 1.000000000000000000, 0.000000000000000000, 0.000000000000000000 ) ) ;
#9001 = EDGE_CURVE ( 'NONE', #13542, #2315, #18943, .T. ) ;
#9002 = DIRECTION ( 'NONE',  ( 0.4999999999999919509, -0.8660254037844432595, -3.491481338843076952E-15 ) ) ;
#9003 = FACE_OUTER_BOUND ( 'NONE', #7660, .T. ) ;
#9004 = LINE ( 'NONE', #15245, #18259 ) ;
#9005 = CARTESIAN_POINT ( 'NONE',  ( 37.78325588002174840, -47.56406379474564972, 283.5832628385307999 ) ) ;
#9006 = EDGE_LOOP ( 'NONE', ( #18104, #1184, #13874 ) ) ;
#9007 = DIRECTION ( 'NONE',  ( 6.982962677686266711E-15, -0.000000000000000000, 1.000000000000000000 ) ) ;
#9008 = CARTESIAN_POINT ( 'NONE',  ( 118.3534152657848608, 114.7431683447366595, 49.99999999999999289 ) ) ;
#9009 = ORIENTED_EDGE ( 'NONE', *, *, #17156, .T. ) ;
#9010 = CIRCLE ( 'NONE', #19444, 106.4288957539801004 ) ;
#9011 = VERTEX_POINT ( 'NONE', #9710 ) ;
#9012 = EDGE_CURVE ( 'NONE', #2414, #12970, #16068, .T. ) ;
#9013 = ORIENTED_EDGE ( 'NONE', *, *, #18489, .T. ) ;
#9014 = CARTESIAN_POINT ( 'NONE',  ( -110.0000000000000142, 275.0000000000000000, 39.99999999999997868 ) ) ;
#9015 = EDGE_LOOP ( 'NONE', ( #18853, #17525, #8895, #9828 ) ) ;
#9016 = CARTESIAN_POINT ( 'NONE',  ( -14.39940464655760799, -76.92888220842480962, 248.9926560891072143 ) ) ;
#9017 = CARTESIAN_POINT ( 'NONE',  ( -3.453261854572979406, -4.581103194069958917, 283.5832628385307999 ) ) ;
#9018 = CARTESIAN_POINT ( 'NONE',  ( 7.500000000000008882, 164.0736214083062805, 60.00000000000000000 ) ) ;
#9019 = CIRCLE ( 'NONE', #1529, 7.500000000000008882 ) ;
#9020 = VECTOR ( 'NONE', #5193, 999.9999999999998863 ) ;
#9021 = PLANE ( 'NONE',  #1117 ) ;
#9022 = LINE ( 'NONE', #10656, #10718 ) ;
#9023 = EDGE_CURVE ( 'NONE', #13898, #10316, #10611, .T. ) ;
#9024 = EDGE_CURVE ( 'NONE', #19819, #11232, #7050, .T. ) ;
#9025 = CARTESIAN_POINT ( 'NONE',  ( 0.000000000000000000, -7.794228634059936489, 4.500000000000017764 ) ) ;
#9026 = EDGE_LOOP ( 'NONE', ( #5940, #13745, #14090 ) ) ;
#9027 = DIRECTION ( 'NONE',  ( 0.000000000000000000, 0.000000000000000000, 1.000000000000000000 ) ) ;
#9028 = CARTESIAN_POINT ( 'NONE',  ( -133.2472142827617461, -69.01451035579515292, 8.943524711593516585 ) ) ;
#9029 = AXIS2_PLACEMENT_3D ( 'NONE', #19197, #4886, #17365 ) ;
#9030 = CARTESIAN_POINT ( 'NONE',  ( 133.8370531740367824, -67.73246766859801937, 0.8536925741625657205 ) ) ;
#9031 = CARTESIAN_POINT ( 'NONE',  ( 51.51682027493064453, -28.15057869795607459, 132.4711112102474146 ) ) ;
#9032 = CARTESIAN_POINT ( 'NONE',  ( -12.14957802882752524, -59.51724408343569905, 293.5832628385307999 ) ) ;
#9033 = CARTESIAN_POINT ( 'NONE',  ( 1.396592535537253342E-14, 0.000000000000000000, 60.00000000000000000 ) ) ;
#9034 = ADVANCED_FACE ( 'NONE', ( #3771 ), #6660, .F. ) ;
#9035 = ORIENTED_EDGE ( 'NONE', *, *, #7995, .F. ) ;
#9036 = LINE ( 'NONE', #12413, #17737 ) ;
#9037 = ADVANCED_FACE ( 'NONE', ( #19135 ), #6947, .T. ) ;
#9038 = CIRCLE ( 'NONE', #15759, 79.75827554147308263 ) ;
#9039 = EDGE_LOOP ( 'NONE', ( #4003, #15197, #12936 ) ) ;
#9040 = VERTEX_POINT ( 'NONE', #9917 ) ;
#9041 = ORIENTED_EDGE ( 'NONE', *, *, #904, .T. ) ;
#9042 = DIRECTION ( 'NONE',  ( -6.982962677686266711E-15, 0.000000000000000000, -1.000000000000000000 ) ) ;
#9043 = CARTESIAN_POINT ( 'NONE',  ( 74.01264520835151473, -25.47058595421579597, 111.4180192758974499 ) ) ;
#9044 = DIRECTION ( 'NONE',  ( 0.000000000000000000, 0.000000000000000000, 1.000000000000000000 ) ) ;
#9045 = ORIENTED_EDGE ( 'NONE', *, *, #17980, .F. ) ;
#9046 = FACE_OUTER_BOUND ( 'NONE', #6970, .T. ) ;
#9047 = CARTESIAN_POINT ( 'NONE',  ( -30.05702882063063086, -50.41613078340792242, 132.4711112102474146 ) ) ;
#9048 = ORIENTED_EDGE ( 'NONE', *, *, #12722, .T. ) ;
#9049 = LINE ( 'NONE', #5895, #17612 ) ;
#9050 = DIRECTION ( 'NONE',  ( -0.1736481776669340504, 0.9848077530122074652, 0.000000000000000000 ) ) ;
#9051 = DIRECTION ( 'NONE',  ( -1.000000000000000000, 0.000000000000000000, 0.000000000000000000 ) ) ;
#9052 = CARTESIAN_POINT ( 'NONE',  ( 42.50000000000000000, 0.000000000000000000, -115.0000000000000000 ) ) ;
#9053 = VECTOR ( 'NONE', #6533, 1000.000000000000000 ) ;
#9054 = AXIS2_PLACEMENT_3D ( 'NONE', #14921, #908, #14531 ) ;
#9055 = UNCERTAINTY_MEASURE_WITH_UNIT (LENGTH_MEASURE( 1.000000000000000082E-05 ), #6659, 'distance_accuracy_value', 'NONE');
#9056 = CIRCLE ( 'NONE', #249, 62.91752772691707207 ) ;
#9057 = CARTESIAN_POINT ( 'NONE',  ( -63.68887634719365565, -147.8252249328922687, 39.99999999999999289 ) ) ;
#9058 = CARTESIAN_POINT ( 'NONE',  ( 41.69438488732684078, 106.8146822993833780, 39.88498244535516335 ) ) ;
#9059 = ORIENTED_EDGE ( 'NONE', *, *, #7912, .T. ) ;
#9060 = EDGE_LOOP ( 'NONE', ( #6432, #11368, #4069, #18346 ) ) ;
#9061 = DIRECTION ( 'NONE',  ( 1.000000000000000000, 0.000000000000000000, 0.000000000000000000 ) ) ;
#9062 = EDGE_LOOP ( 'NONE', ( #14196, #1809, #1256, #20061 ) ) ;
#9063 = ORIENTED_EDGE ( 'NONE', *, *, #15369, .T. ) ;
#9064 = LINE ( 'NONE', #6014, #13808 ) ;
#9065 = ORIENTED_EDGE ( 'NONE', *, *, #7854, .F. ) ;
#9066 = ORIENTED_EDGE ( 'NONE', *, *, #11425, .F. ) ;
#9067 = AXIS2_PLACEMENT_3D ( 'NONE', #4144, #5687, #10370 ) ;
#9068 = DIRECTION ( 'NONE',  ( 0.000000000000000000, 0.000000000000000000, 1.000000000000000000 ) ) ;
#9069 = B_SPLINE_CURVE_WITH_KNOTS ( 'NONE', 3,
 ( #2516, #8745, #14989, #18164, #4146, #16635 ),
 .UNSPECIFIED., .F., .F.,
 ( 4, 2, 4 ),
 ( 2.380730968224042413E-07, 0.002629065763328366535, 0.005257893453559910578 ),
 .UNSPECIFIED. ) ;
#9070 = VECTOR ( 'NONE', #10641, 1000.000000000000227 ) ;
#9071 =( NAMED_UNIT ( * ) PLANE_ANGLE_UNIT ( ) SI_UNIT ( $, .RADIAN. ) );
#9072 = DIRECTION ( 'NONE',  ( 1.000000000000000000, 0.000000000000000000, 0.000000000000000000 ) ) ;
#9073 = ORIENTED_EDGE ( 'NONE', *, *, #3534, .F. ) ;
#9074 = LINE ( 'NONE', #7542, #6742 ) ;
#9075 = CARTESIAN_POINT ( 'NONE',  ( -159.9599531637108782, -36.50981547337168109, 60.00000000000000000 ) ) ;
#9076 = VERTEX_POINT ( 'NONE', #14524 ) ;
#9077 = FACE_OUTER_BOUND ( 'NONE', #10588, .T. ) ;
#9078 = CARTESIAN_POINT ( 'NONE',  ( 70.38703763562273252, -92.47916748300480094, 14.88498244535495907 ) ) ;
#9079 = EDGE_CURVE ( 'NONE', #12028, #2362, #8180, .T. ) ;
#9080 = CARTESIAN_POINT ( 'NONE',  ( -27.49999999999998934, 0.000000000000000000, 127.7817459305202448 ) ) ;
#9081 = VECTOR ( 'NONE', #13904, 1000.000000000000000 ) ;
#9082 = CARTESIAN_POINT ( 'NONE',  ( -29.99999999999887379, 275.0000000000000000, 4.999999999999158007 ) ) ;
#9083 = FACE_OUTER_BOUND ( 'NONE', #3516, .T. ) ;
#9084 = CARTESIAN_POINT ( 'NONE',  ( -109.4759482221338516, 87.26817553548865192, 40.00000000000000000 ) ) ;
#9085 = AXIS2_PLACEMENT_3D ( 'NONE', #18237, #10448, #2692 ) ;
#9086 = VERTEX_POINT ( 'NONE', #19525 ) ;
#9087 = AXIS2_PLACEMENT_3D ( 'NONE', #3395, #11463, #114 ) ;
#9088 = FACE_BOUND ( 'NONE', #13458, .T. ) ;
#9089 = CARTESIAN_POINT ( 'NONE',  ( -12.23146955673647618, -77.31114765718484705, 132.4711112102474146 ) ) ;
#9090 = ORIENTED_EDGE ( 'NONE', *, *, #6647, .F. ) ;
#9091 = VERTEX_POINT ( 'NONE', #16168 ) ;
#9092 = CARTESIAN_POINT ( 'NONE',  ( -97.34896704141375778, -115.5410409671962384, 29.72470138523284788 ) ) ;
#9093 = EDGE_CURVE ( 'NONE', #17191, #11184, #5416, .T. ) ;
#9094 = ORIENTED_EDGE ( 'NONE', *, *, #18159, .F. ) ;
#9095 = EDGE_CURVE ( 'NONE', #6917, #295, #16192, .T. ) ;
#9096 = CARTESIAN_POINT ( 'NONE',  ( 0.000000000000000000, 0.000000000000000000, -49.99999999999999289 ) ) ;
#9097 = ORIENTED_EDGE ( 'NONE', *, *, #7004, .F. ) ;
#9098 = CARTESIAN_POINT ( 'NONE',  ( 95.52811048055005472, -116.1520858409644745, 8.469523593983353749 ) ) ;
#9099 = DIRECTION ( 'NONE',  ( -6.982962677686266711E-15, 0.000000000000000000, -1.000000000000000000 ) ) ;
#9100 = CIRCLE ( 'NONE', #11077, 79.75827554147308263 ) ;
#9101 = VECTOR ( 'NONE', #6563, 1000.000000000000000 ) ;
#9102 = EDGE_CURVE ( 'NONE', #4859, #6447, #12575, .T. ) ;
#9103 = CARTESIAN_POINT ( 'NONE',  ( -54.86954475316242252, 20.84572577951219330, 132.4711112102474146 ) ) ;
#9104 = DIRECTION ( 'NONE',  ( -0.3420201433256601642, -0.9396926207859114255, 0.000000000000000000 ) ) ;
#9105 = FACE_OUTER_BOUND ( 'NONE', #2649, .T. ) ;
#9106 = DIRECTION ( 'NONE',  ( 1.000000000000000000, 0.000000000000000000, 0.000000000000000000 ) ) ;
#9107 = DIRECTION ( 'NONE',  ( 0.000000000000000000, 0.000000000000000000, 1.000000000000000000 ) ) ;
#9108 = CARTESIAN_POINT ( 'NONE',  ( 95.42019791136713991, -116.1393900958193655, 32.10275980689200992 ) ) ;
#9109 = VERTEX_POINT ( 'NONE', #10016 ) ;
#9110 = AXIS2_PLACEMENT_3D ( 'NONE', #5546, #1028, #7184 ) ;
#9111 = CARTESIAN_POINT ( 'NONE',  ( 59.30917539369505675, -13.12769224524051559, 293.5832628385307999 ) ) ;
#9112 = CARTESIAN_POINT ( 'NONE',  ( 12.78021302872850562, -77.21438937758507848, 132.4711112102474146 ) ) ;
#9113 = EDGE_LOOP ( 'NONE', ( #11417, #5922, #14744, #10485 ) ) ;
#9114 = AXIS2_PLACEMENT_3D ( 'NONE', #15838, #4585, #7745 ) ;
#9115 = ORIENTED_EDGE ( 'NONE', *, *, #12344, .T. ) ;
#9116 = DIRECTION ( 'NONE',  ( 1.000000000000000000, 0.000000000000000000, 0.000000000000000000 ) ) ;
#9117 = EDGE_CURVE ( 'NONE', #3818, #14077, #9654, .T. ) ;
#9118 = EDGE_CURVE ( 'NONE', #11697, #11236, #11601, .T. ) ;
#9119 = ORIENTED_EDGE ( 'NONE', *, *, #20172, .T. ) ;
#9120 = ADVANCED_FACE ( 'NONE', ( #19333 ), #11351, .T. ) ;
#9121 = FACE_BOUND ( 'NONE', #4135, .T. ) ;
#9122 = VERTEX_POINT ( 'NONE', #11244 ) ;
#9123 = CARTESIAN_POINT ( 'NONE',  ( 50.37374754117451658, -141.2886604036503115, 60.00000000000000000 ) ) ;
#9124 = CARTESIAN_POINT ( 'NONE',  ( 132.8201933467846061, -84.36756360499407492, 0.9536901868107962033 ) ) ;
#9125 = LINE ( 'NONE', #2690, #8734 ) ;
#9126 = CARTESIAN_POINT ( 'NONE',  ( -53.78543575132151489, -32.64570716507521553, 132.4711112102474146 ) ) ;
#9127 = CARTESIAN_POINT ( 'NONE',  ( -32.50000000000000000, 3.980102097228898626E-15, -105.0000000000000142 ) ) ;
#9128 = DIRECTION ( 'NONE',  ( 0.000000000000000000, 0.000000000000000000, 1.000000000000000000 ) ) ;
#9129 = CIRCLE ( 'NONE', #1915, 77.50000000000000000 ) ;
#9130 = CIRCLE ( 'NONE', #14372, 15.91767397667355155 ) ;
#9131 = ORIENTED_EDGE ( 'NONE', *, *, #61, .T. ) ;
#9132 = CARTESIAN_POINT ( 'NONE',  ( 9.381844291199747943, -57.94128254008187184, 112.0427633081291816 ) ) ;
#9133 = DIRECTION ( 'NONE',  ( -1.000000000000000000, 0.000000000000000000, 0.000000000000000000 ) ) ;
#9134 = EDGE_CURVE ( 'NONE', #5555, #9722, #704, .T. ) ;
#9135 = CARTESIAN_POINT ( 'NONE',  ( 128.0993248974582741, -78.05374007934287306, -8.252068616993026851 ) ) ;
#9136 = CARTESIAN_POINT ( 'NONE',  ( -170.2125097089225960, -199.3942630591407692, 0.000000000000000000 ) ) ;
#9137 = CARTESIAN_POINT ( 'NONE',  ( 0.000000000000000000, 0.000000000000000000, 283.5832628385307999 ) ) ;
#9138 = CARTESIAN_POINT ( 'NONE',  ( -134.3287459046936760, -75.81846210759933058, 35.02824617995954526 ) ) ;
#9139 = ORIENTED_EDGE ( 'NONE', *, *, #15416, .F. ) ;
#9140 = DIRECTION ( 'NONE',  ( -0.000000000000000000, -0.000000000000000000, 1.000000000000000000 ) ) ;
#9141 = AXIS2_PLACEMENT_3D ( 'NONE', #2087, #14560, #6491 ) ;
#9142 = ORIENTED_EDGE ( 'NONE', *, *, #9643, .F. ) ;
#9143 = EDGE_CURVE ( 'NONE', #18380, #1203, #8651, .T. ) ;
#9144 = EDGE_CURVE ( 'NONE', #20089, #13453, #16830, .T. ) ;
#9145 = EDGE_CURVE ( 'NONE', #11033, #13667, #2345, .T. ) ;
#9146 = EDGE_CURVE ( 'NONE', #15549, #17410, #811, .T. ) ;
#9147 = ORIENTED_EDGE ( 'NONE', *, *, #4775, .F. ) ;
#9148 = EDGE_LOOP ( 'NONE', ( #11780, #15203, #8368, #7502 ) ) ;
#9149 = CARTESIAN_POINT ( 'NONE',  ( -137.5033450361952418, -27.36572496882791583, 26.67424988177857159 ) ) ;
#9150 = DIRECTION ( 'NONE',  ( 0.6427876096865458022, -0.7660444431189726844, 0.000000000000000000 ) ) ;
#9151 = DIRECTION ( 'NONE',  ( 0.000000000000000000, 0.000000000000000000, 1.000000000000000000 ) ) ;
#9152 = EDGE_LOOP ( 'NONE', ( #7355, #16352, #16009, #10670, #7115, #16058 ) ) ;
#9153 = ADVANCED_FACE ( 'NONE', ( #8675 ), #898, .T. ) ;
#9154 = CARTESIAN_POINT ( 'NONE',  ( -130.9868171408399462, -91.88282611735537841, 50.00000000000000000 ) ) ;
#9155 = CARTESIAN_POINT ( 'NONE',  ( 116.5881606921954017, -25.59923667990641150, 14.88498244535463755 ) ) ;
#9156 = VERTEX_POINT ( 'NONE', #5815 ) ;
#9157 = CARTESIAN_POINT ( 'NONE',  ( 0.000000000000000000, 0.000000000000000000, 0.000000000000000000 ) ) ;
#9158 = EDGE_CURVE ( 'NONE', #2090, #5714, #7244, .T. ) ;
#9159 = CARTESIAN_POINT ( 'NONE',  ( 20.84572577951164618, 54.86954475316263569, 248.9926560891072143 ) ) ;
#9160 = CARTESIAN_POINT ( 'NONE',  ( 170.2125097089226244, -199.3942630591406839, 0.000000000000000000 ) ) ;
#9161 = CARTESIAN_POINT ( 'NONE',  ( 32.61983739937763005, 51.24071425735591845, 283.5832628385307999 ) ) ;
#9162 = VECTOR ( 'NONE', #6212, 1000.000000000000000 ) ;
#9163 = DIRECTION ( 'NONE',  ( 0.3420201433256630508, 0.9396926207859104263, 0.000000000000000000 ) ) ;
#9164 = CARTESIAN_POINT ( 'NONE',  ( 130.0656023054208106, -74.72982709287474279, 46.44206350853437471 ) ) ;
#9165 = FACE_OUTER_BOUND ( 'NONE', #5071, .T. ) ;
#9166 = ORIENTED_EDGE ( 'NONE', *, *, #14113, .F. ) ;
#9167 = ORIENTED_EDGE ( 'NONE', *, *, #3381, .T. ) ;
#9168 = DIRECTION ( 'NONE',  ( 1.000000000000000000, 0.000000000000000000, 0.000000000000000000 ) ) ;
#9169 = ORIENTED_EDGE ( 'NONE', *, *, #11535, .F. ) ;
#9170 = ORIENTED_EDGE ( 'NONE', *, *, #4754, .T. ) ;
#9171 = DIRECTION ( 'NONE',  ( -0.000000000000000000, -0.000000000000000000, 1.000000000000000000 ) ) ;
#9172 = VERTEX_POINT ( 'NONE', #4272 ) ;
#9173 = CARTESIAN_POINT ( 'NONE',  ( 79.05640494598117129, -127.4758205975433327, 60.00000000000000000 ) ) ;
#9174 = CIRCLE ( 'NONE', #12772, 3.224098631618460775 ) ;
#9175 = EDGE_CURVE ( 'NONE', #9484, #15959, #18190, .T. ) ;
#9176 = CARTESIAN_POINT ( 'NONE',  ( 0.3570196857253401523, -6.047589086024969696, 7.525268439705683932 ) ) ;
#9177 = CARTESIAN_POINT ( 'NONE',  ( -163.5019688434124419, -20.99123081650240863, 39.99999999999999289 ) ) ;
#9178 = CARTESIAN_POINT ( 'NONE',  ( 0.000000000000000000, 0.000000000000000000, 132.4711112102474146 ) ) ;
#9179 = ORIENTED_EDGE ( 'NONE', *, *, #7007, .F. ) ;
#9180 = DIRECTION ( 'NONE',  ( 6.982962677686266711E-15, -0.000000000000000000, 1.000000000000000000 ) ) ;
#9181 = DIRECTION ( 'NONE',  ( 1.000000000000000000, 0.000000000000000000, 0.000000000000000000 ) ) ;
#9182 = ORIENTED_EDGE ( 'NONE', *, *, #16863, .T. ) ;
#9183 = VECTOR ( 'NONE', #5163, 1000.000000000000000 ) ;
#9184 = DIRECTION ( 'NONE',  ( 1.000000000000000000, 0.000000000000000000, -0.000000000000000000 ) ) ;
#9185 = CARTESIAN_POINT ( 'NONE',  ( 5.693982670708947147, -0.7000608949449556029, 293.5832628385307999 ) ) ;
#9186 = CARTESIAN_POINT ( 'NONE',  ( 75.91068486117727332, -120.9436655338208340, 49.99999999999999289 ) ) ;
#9187 = CIRCLE ( 'NONE', #1349, 150.0000000000000284 ) ;
#9188 = CARTESIAN_POINT ( 'NONE',  ( -23.23469325536255070, -13.41455640552162443, 39.88498244535561810 ) ) ;
#9189 = CARTESIAN_POINT ( 'NONE',  ( -132.1979689506645741, -87.16940599486621011, 39.62925165859044796 ) ) ;
#9190 = VECTOR ( 'NONE', #3808, 1000.000000000000114 ) ;
#9191 = CARTESIAN_POINT ( 'NONE',  ( -91.86817182112051228, 105.6448302045327523, 34.94516124885768704 ) ) ;
#9192 = ORIENTED_EDGE ( 'NONE', *, *, #16479, .T. ) ;
#9193 = CARTESIAN_POINT ( 'NONE',  ( 7.500000000000001776, 60.00000000000000000, -115.0000000000000000 ) ) ;
#9194 = DIRECTION ( 'NONE',  ( 0.9848077530122073542, 0.1736481776669340227, 0.000000000000000000 ) ) ;
#9195 = VERTEX_POINT ( 'NONE', #10401 ) ;
#9196 = ORIENTED_EDGE ( 'NONE', *, *, #16366, .F. ) ;
#9197 = CARTESIAN_POINT ( 'NONE',  ( -97.49999999999997158, -133.9542832461778232, 30.37260543920541878 ) ) ;
#9198 = EDGE_LOOP ( 'NONE', ( #10649, #3894, #18779 ) ) ;
#9199 = EDGE_CURVE ( 'NONE', #6070, #1994, #501, .T. ) ;
#9200 = DIRECTION ( 'NONE',  ( -1.000000000000000000, 0.000000000000000000, 0.000000000000000000 ) ) ;
#9201 = FACE_OUTER_BOUND ( 'NONE', #9560, .T. ) ;
#9202 = ORIENTED_EDGE ( 'NONE', *, *, #6252, .T. ) ;
#9203 = CARTESIAN_POINT ( 'NONE',  ( 98.53720805795899196, -132.5762351826696204, 5.561479031436848075 ) ) ;
#9204 = CARTESIAN_POINT ( 'NONE',  ( -53.40063514825077107, -28.94886449118923011, 283.5832628385307999 ) ) ;
#9205 = AXIS2_PLACEMENT_3D ( 'NONE', #9570, #9668, #1797 ) ;
#9206 = DIRECTION ( 'NONE',  ( 6.982962677686266711E-15, 0.000000000000000000, 1.000000000000000000 ) ) ;
#9207 = FACE_OUTER_BOUND ( 'NONE', #686, .T. ) ;
#9208 = EDGE_LOOP ( 'NONE', ( #16435, #7532, #2009, #10544 ) ) ;
#9209 = EDGE_CURVE ( 'NONE', #4654, #6858, #5081, .T. ) ;
#9210 = DIRECTION ( 'NONE',  ( 6.982962677686266711E-15, -0.000000000000000000, 1.000000000000000000 ) ) ;
#9211 = FACE_OUTER_BOUND ( 'NONE', #5498, .T. ) ;
#9212 = DIRECTION ( 'NONE',  ( 1.000000000000000000, 0.000000000000000000, 0.000000000000000000 ) ) ;
#9213 = CARTESIAN_POINT ( 'NONE',  ( 85.51233150139638894, -123.2383548749651254, 41.61296411234719272 ) ) ;
#9214 = EDGE_LOOP ( 'NONE', ( #17946, #12312, #2180, #17045 ) ) ;
#9215 = DIRECTION ( 'NONE',  ( 1.000000000000000000, 0.000000000000000000, -6.994638739193269649E-15 ) ) ;
#9216 = CARTESIAN_POINT ( 'NONE',  ( -136.4994460260996902, -31.11111111111111427, 27.86436879316430648 ) ) ;
#9217 = VERTEX_POINT ( 'NONE', #4374 ) ;
#9218 = ORIENTED_EDGE ( 'NONE', *, *, #9967, .T. ) ;
#9219 = APPLICATION_PROTOCOL_DEFINITION ( 'draft international standard', 'automotive_design', 1998, #453 ) ;
#9220 = VECTOR ( 'NONE', #15489, 1000.000000000000000 ) ;
#9221 = AXIS2_PLACEMENT_3D ( 'NONE', #6158, #1958, #3186 ) ;
#9222 = VERTEX_POINT ( 'NONE', #2747 ) ;
#9223 = ADVANCED_FACE ( 'NONE', ( #3967 ), #19715, .F. ) ;
#9224 = DIRECTION ( 'NONE',  ( 1.000000000000000000, 0.000000000000000000, 0.000000000000000000 ) ) ;
#9225 = EDGE_CURVE ( 'NONE', #2759, #1374, #5723, .T. ) ;
#9226 = DIRECTION ( 'NONE',  ( 1.000000000000000000, 3.320906611023727849E-16, 0.000000000000000000 ) ) ;
#9227 = VERTEX_POINT ( 'NONE', #12033 ) ;
#9228 = VECTOR ( 'NONE', #16077, 1000.000000000000000 ) ;
#9229 = DIRECTION ( 'NONE',  ( -0.8830229359480288309, -0.4693298356057531984, 0.000000000000000000 ) ) ;
#9230 = DIRECTION ( 'NONE',  ( -1.000000000000000000, -0.000000000000000000, -0.000000000000000000 ) ) ;
#9231 = AXIS2_PLACEMENT_3D ( 'NONE', #10743, #5953, #6059 ) ;
#9232 = LINE ( 'NONE', #4930, #8537 ) ;
#9233 = CARTESIAN_POINT ( 'NONE',  ( -95.44915936929146483, -116.0550301922269085, 32.61437126001344922 ) ) ;
#9234 = FACE_OUTER_BOUND ( 'NONE', #18816, .T. ) ;
#9235 = CARTESIAN_POINT ( 'NONE',  ( 71.18887634719571622, -147.8252249328912740, 39.99999999999999289 ) ) ;
#9236 = DIRECTION ( 'NONE',  ( 0.000000000000000000, 0.000000000000000000, 1.000000000000000000 ) ) ;
#9237 = CARTESIAN_POINT ( 'NONE',  ( -134.9140359355702685, -65.56103033672289371, 6.267746957543315567 ) ) ;
#9238 = EDGE_CURVE ( 'NONE', #4139, #13695, #19620, .T. ) ;
#9239 = CARTESIAN_POINT ( 'NONE',  ( 128.7754324793921228, -76.93177152330439128, -7.719765474015907181 ) ) ;
#9240 = CIRCLE ( 'NONE', #4678, 10.00000000000000888 ) ;
#9241 = AXIS2_PLACEMENT_3D ( 'NONE', #16235, #17972, #867 ) ;
#9242 = EDGE_CURVE ( 'NONE', #10879, #10504, #18296, .T. ) ;
#9243 = FACE_OUTER_BOUND ( 'NONE', #14368, .T. ) ;
#9244 = CARTESIAN_POINT ( 'NONE',  ( -132.0512179319685515, -87.77725330520023306, 39.71072694138295844 ) ) ;
#9245 = ORIENTED_EDGE ( 'NONE', *, *, #2365, .F. ) ;
#9246 = ADVANCED_FACE ( 'NONE', ( #14912 ), #4172, .F. ) ;
#9247 = CARTESIAN_POINT ( 'NONE',  ( 58.63718168490485283, 22.81000261549389307, 132.4711112102474146 ) ) ;
#9248 = AXIS2_PLACEMENT_3D ( 'NONE', #15102, #1082, #7330 ) ;
#9249 = CIRCLE ( 'NONE', #12511, 60.74260934110282051 ) ;
#9250 = ORIENTED_EDGE ( 'NONE', *, *, #5302, .T. ) ;
#9251 = ORIENTED_EDGE ( 'NONE', *, *, #9724, .T. ) ;
#9252 = EDGE_CURVE ( 'NONE', #6551, #5955, #9313, .T. ) ;
#9253 = EDGE_CURVE ( 'NONE', #19254, #17576, #1311, .T. ) ;
#9254 = CIRCLE ( 'NONE', #15132, 3.224098631618459443 ) ;
#9255 = CIRCLE ( 'NONE', #12843, 7.500000000000000000 ) ;
#9256 = ORIENTED_EDGE ( 'NONE', *, *, #9242, .T. ) ;
#9257 = FACE_OUTER_BOUND ( 'NONE', #19991, .T. ) ;
#9258 = LINE ( 'NONE', #18464, #2875 ) ;
#9259 = VERTEX_POINT ( 'NONE', #18092 ) ;
#9260 = DIRECTION ( 'NONE',  ( -1.000000000000000000, 0.000000000000000000, 0.000000000000000000 ) ) ;
#9261 = CARTESIAN_POINT ( 'NONE',  ( 41.02212542604613077, 44.79787735033405482, 293.5832628385307999 ) ) ;
#9262 = ORIENTED_EDGE ( 'NONE', *, *, #764, .T. ) ;
#9263 = DIRECTION ( 'NONE',  ( 1.000000000000000000, 0.000000000000000000, 0.000000000000000000 ) ) ;
#9264 = LINE ( 'NONE', #18689, #17875 ) ;
#9265 = CARTESIAN_POINT ( 'NONE',  ( 48.17959877923549072, 36.99514631729036296, 293.5832628385307999 ) ) ;
#9266 = AXIS2_PLACEMENT_3D ( 'NONE', #17300, #9708, #1733 ) ;
#9267 = EDGE_CURVE ( 'NONE', #17702, #8089, #15211, .T. ) ;
#9268 = DIRECTION ( 'NONE',  ( -0.9993852124581887875, 0.03505990758545545621, 0.000000000000000000 ) ) ;
#9269 = CARTESIAN_POINT ( 'NONE',  ( -31.77296517111735596, -51.77251465595229263, 293.5832628385307999 ) ) ;
#9270 = EDGE_CURVE ( 'NONE', #15648, #7108, #9973, .T. ) ;
#9271 = CARTESIAN_POINT ( 'NONE',  ( 134.9866372717144998, -65.41115948451921724, 32.98563192608333594 ) ) ;
#9272 = LINE ( 'NONE', #20108, #216 ) ;
#9273 = EDGE_LOOP ( 'NONE', ( #15004, #10275, #15041, #215 ) ) ;
#9274 = VERTEX_POINT ( 'NONE', #19922 ) ;
#9275 = VERTEX_POINT ( 'NONE', #18398 ) ;
#9276 = AXIS2_PLACEMENT_3D ( 'NONE', #11068, #11171, #17436 ) ;
#9277 = ORIENTED_EDGE ( 'NONE', *, *, #10163, .F. ) ;
#9278 = LINE ( 'NONE', #4893, #16456 ) ;
#9279 = EDGE_CURVE ( 'NONE', #19819, #6720, #11723, .T. ) ;
#9280 = AXIS2_PLACEMENT_3D ( 'NONE', #16462, #2442, #8673 ) ;
#9281 = ORIENTED_EDGE ( 'NONE', *, *, #2241, .F. ) ;
#9282 = DIRECTION ( 'NONE',  ( -0.1736481776669306920, 0.9848077530122080203, 0.000000000000000000 ) ) ;
#9283 = DIRECTION ( 'NONE',  ( 0.000000000000000000, 1.000000000000000000, 0.000000000000000000 ) ) ;
#9284 = DIRECTION ( 'NONE',  ( 1.000000000000000000, 0.000000000000000000, 0.000000000000000000 ) ) ;
#9285 = DIRECTION ( 'NONE',  ( 6.982962677686266711E-15, -0.000000000000000000, 1.000000000000000000 ) ) ;
#9286 = ORIENTED_EDGE ( 'NONE', *, *, #11719, .F. ) ;
#9287 = DIRECTION ( 'NONE',  ( 1.000000000000000000, 0.000000000000000000, -6.994638739193275171E-15 ) ) ;
#9288 = CARTESIAN_POINT ( 'NONE',  ( 78.26059000578310076, 1.379293853802574077, 132.4711112102474146 ) ) ;
#9289 = ORIENTED_EDGE ( 'NONE', *, *, #11773, .T. ) ;
#9290 = PRODUCT_DEFINITION_CONTEXT ( 'detailed design', #10235, 'design' ) ;
#9291 = DIRECTION ( 'NONE',  ( 0.7660444431189749048, 0.6427876096865430267, -0.000000000000000000 ) ) ;
#9292 = DIRECTION ( 'NONE',  ( -0.000000000000000000, -0.000000000000000000, 1.000000000000000000 ) ) ;
#9293 = ADVANCED_FACE ( 'NONE', ( #8773 ), #15016, .F. ) ;
#9294 = AXIS2_PLACEMENT_3D ( 'NONE', #14119, #12473, #18429 ) ;
#9295 = PLANE ( 'NONE',  #3440 ) ;
#9296 = VECTOR ( 'NONE', #11519, 1000.000000000000000 ) ;
#9297 = DIRECTION ( 'NONE',  ( 0.000000000000000000, 0.000000000000000000, 1.000000000000000000 ) ) ;
#9298 = CARTESIAN_POINT ( 'NONE',  ( 59.30917539369505675, -13.12769224524051559, 283.5832628385307999 ) ) ;
#9299 = CARTESIAN_POINT ( 'NONE',  ( -76.58875299708743967, 117.1931663892607958, 15.45866710248154519 ) ) ;
#9300 = EDGE_CURVE ( 'NONE', #11632, #3495, #15323, .T. ) ;
#9301 = EDGE_LOOP ( 'NONE', ( #18979, #15667, #3502, #19728 ) ) ;
#9302 = DIRECTION ( 'NONE',  ( -6.982962677686266711E-15, 0.000000000000000000, -1.000000000000000000 ) ) ;
#9303 = ORIENTED_EDGE ( 'NONE', *, *, #19544, .T. ) ;
#9304 = VERTEX_POINT ( 'NONE', #15532 ) ;
#9305 = CARTESIAN_POINT ( 'NONE',  ( 28.63313560863472063, -51.23821591265105013, 110.9660488491356887 ) ) ;
#9306 = AXIS2_PLACEMENT_3D ( 'NONE', #1100, #12039, #12350 ) ;
#9307 = ORIENTED_EDGE ( 'NONE', *, *, #20115, .F. ) ;
#9308 = CARTESIAN_POINT ( 'NONE',  ( -139.4006145564613917, 50.16213250608596042, -22.20134617928383491 ) ) ;
#9309 = CARTESIAN_POINT ( 'NONE',  ( 12.24586475280392506, -24.22555452564823497, 14.88498244535536585 ) ) ;
#9310 = EDGE_LOOP ( 'NONE', ( #2318, #1723, #1662, #5574 ) ) ;
#9311 = CARTESIAN_POINT ( 'NONE',  ( 99.76899065921492138, -130.8788316638307379, 3.647911195597622225 ) ) ;
#9312 = DIRECTION ( 'NONE',  ( -0.000000000000000000, -0.000000000000000000, 1.000000000000000000 ) ) ;
#9313 = CIRCLE ( 'NONE', #17168, 15.91767397667354444 ) ;
#9314 = DIRECTION ( 'NONE',  ( 0.7660444431189707970, 0.6427876096865481337, 0.000000000000000000 ) ) ;
#9315 = CARTESIAN_POINT ( 'NONE',  ( 50.37374754117451658, -141.2886604036503115, 60.00000000000000000 ) ) ;
#9316 = ORIENTED_EDGE ( 'NONE', *, *, #17991, .T. ) ;
#9317 = CARTESIAN_POINT ( 'NONE',  ( 60.83768308848376449, -49.24833719034207036, 248.9926560891072143 ) ) ;
#9318 = VECTOR ( 'NONE', #3515, 1000.000000000000227 ) ;
#9319 = DIRECTION ( 'NONE',  ( -1.000000000000000000, 0.000000000000000000, 0.000000000000000000 ) ) ;
#9320 = LINE ( 'NONE', #15563, #11822 ) ;
#9321 = CARTESIAN_POINT ( 'NONE',  ( 98.17258311761688105, -133.0662226711789629, 33.62401363155364464 ) ) ;
#9322 = VERTEX_POINT ( 'NONE', #13885 ) ;
#9323 = DIRECTION ( 'NONE',  ( 1.000000000000000000, 0.000000000000000000, 0.000000000000000000 ) ) ;
#9324 = DIRECTION ( 'NONE',  ( -0.4338837391175509040, -0.9009688679024224767, 0.000000000000000000 ) ) ;
#9325 = VERTEX_POINT ( 'NONE', #15425 ) ;
#9326 = ORIENTED_EDGE ( 'NONE', *, *, #17165, .T. ) ;
#9327 = ORIENTED_EDGE ( 'NONE', *, *, #5603, .T. ) ;
#9328 = AXIS2_PLACEMENT_3D ( 'NONE', #11449, #510, #6753 ) ;
#9329 = ORIENTED_EDGE ( 'NONE', *, *, #14484, .T. ) ;
#9330 = CARTESIAN_POINT ( 'NONE',  ( -98.50852301078386120, -132.6154683359945636, 5.603543560907854548 ) ) ;
#9331 = FACE_BOUND ( 'NONE', #10472, .T. ) ;
#9332 = ORIENTED_EDGE ( 'NONE', *, *, #9355, .T. ) ;
#9333 = CARTESIAN_POINT ( 'NONE',  ( 37.78325588002174840, -47.56406379474564972, 283.5832628385307999 ) ) ;
#9334 = LINE ( 'NONE', #3204, #19088 ) ;
#9335 = CARTESIAN_POINT ( 'NONE',  ( 28.06584155524102187, -53.86996498385662591, 283.5832628385307999 ) ) ;
#9336 = CARTESIAN_POINT ( 'NONE',  ( -85.13411715130405355, -123.5004392096852683, 41.04246620030852455 ) ) ;
#9337 = DIRECTION ( 'NONE',  ( 0.000000000000000000, 0.000000000000000000, 1.000000000000000000 ) ) ;
#9338 = DIRECTION ( 'NONE',  ( -0.000000000000000000, -0.000000000000000000, 1.000000000000000000 ) ) ;
#9339 = VECTOR ( 'NONE', #19793, 1000.000000000000114 ) ;
#9340 = LINE ( 'NONE', #4322, #3292 ) ;
#9341 = PLANE ( 'NONE',  #12587 ) ;
#9342 = CARTESIAN_POINT ( 'NONE',  ( 132.4144148199947324, -86.21736781322083232, 0.5493819109983639759 ) ) ;
#9343 = CARTESIAN_POINT ( 'NONE',  ( 19.63382932406824466, 18.38657833536341357, 14.88498244535531256 ) ) ;
#9344 = CARTESIAN_POINT ( 'NONE',  ( -23.22641211976288389, -56.12662799072081299, 293.5832628385307999 ) ) ;
#9345 = CARTESIAN_POINT ( 'NONE',  ( -133.2581445365307786, -82.18041427990793579, 38.38389406139176430 ) ) ;
#9346 = EDGE_CURVE ( 'NONE', #15860, #14685, #15744, .T. ) ;
#9347 = ORIENTED_EDGE ( 'NONE', *, *, #13519, .F. ) ;
#9348 = AXIS2_PLACEMENT_3D ( 'NONE', #7643, #6024, #20123 ) ;
#9349 = LINE ( 'NONE', #10875, #9220 ) ;
#9350 = EDGE_LOOP ( 'NONE', ( #10799, #8419 ) ) ;
#9351 = VERTEX_POINT ( 'NONE', #20124 ) ;
#9352 = CLOSED_SHELL ( 'NONE', ( #14955, #12751, #8723, #4009, #18661, #9730, #1376, #1542, #11651, #13454, #13509, #5260, #17413, #18480, #6255, #13588, #5263, #11014, #17863, #9657, #15655, #8120, #2926, #19659, #15607, #7278, #1480 ) ) ;
#9353 = EDGE_CURVE ( 'NONE', #17450, #13065, #16963, .T. ) ;
#9354 = ORIENTED_EDGE ( 'NONE', *, *, #9409, .F. ) ;
#9355 = EDGE_CURVE ( 'NONE', #9886, #9122, #2274, .T. ) ;
#9356 = CARTESIAN_POINT ( 'NONE',  ( -143.9003822582011765, -15.47344326723975882, 13.71750472807623211 ) ) ;
#9357 = EDGE_CURVE ( 'NONE', #9351, #8683, #20025, .T. ) ;
#9358 = CIRCLE ( 'NONE', #553, 62.91752772691707207 ) ;
#9359 = LINE ( 'NONE', #8023, #12542 ) ;
#9360 = PLANE ( 'NONE',  #12334 ) ;
#9361 = ORIENTED_EDGE ( 'NONE', *, *, #3614, .T. ) ;
#9362 = CARTESIAN_POINT ( 'NONE',  ( -32.50000000000000000, 0.000000000000000000, -40.00000000000000000 ) ) ;
#9363 = DIRECTION ( 'NONE',  ( 0.000000000000000000, 0.000000000000000000, -1.000000000000000000 ) ) ;
#9364 = CARTESIAN_POINT ( 'NONE',  ( -78.68887634719368407, -147.8252249328922687, 49.99999999999999289 ) ) ;
#9365 = CARTESIAN_POINT ( 'NONE',  ( 163.5019688434126977, -20.99123081650019884, 60.00000000000000000 ) ) ;
#9366 = DIRECTION ( 'NONE',  ( 0.3747554100459959958, 0.9271237148521535021, 0.000000000000000000 ) ) ;
#9367 = DIRECTION ( 'NONE',  ( -6.982962677686266711E-15, 0.000000000000000000, -1.000000000000000000 ) ) ;
#9368 = AXIS2_PLACEMENT_3D ( 'NONE', #19412, #5589, #10097 ) ;
#9369 = EDGE_CURVE ( 'NONE', #1970, #5595, #1714, .T. ) ;
#9370 = ORIENTED_EDGE ( 'NONE', *, *, #12775, .F. ) ;
#9371 = VECTOR ( 'NONE', #7265, 1000.000000000000000 ) ;
#9372 = PLANE ( 'NONE',  #264 ) ;
#9373 = CARTESIAN_POINT ( 'NONE',  ( 120.7779226595530986, 102.2982297021113141, 49.99999999999999289 ) ) ;
#9374 = EDGE_LOOP ( 'NONE', ( #19782, #19965, #5937, #17993 ) ) ;
#9376 = VERTEX_POINT ( 'NONE', #18495 ) ;
#9375 = AXIS2_PLACEMENT_3D ( 'NONE', #10839, #20058, #9319 ) ;
#9377 = ORIENTED_EDGE ( 'NONE', *, *, #1371, .F. ) ;
#9378 = VERTEX_POINT ( 'NONE', #12342 ) ;
#9379 = CARTESIAN_POINT ( 'NONE',  ( 0.000000000000000000, 0.000000000000000000, -105.0000000000000142 ) ) ;
#9380 = EDGE_CURVE ( 'NONE', #698, #3700, #9391, .T. ) ;
#9381 = ORIENTED_EDGE ( 'NONE', *, *, #6132, .T. ) ;
#9382 = CARTESIAN_POINT ( 'NONE',  ( 20.84572577951164618, 54.86954475316263569, 111.4180192758974499 ) ) ;
#9383 = EDGE_CURVE ( 'NONE', #1375, #20213, #4475, .T. ) ;
#9384 = ADVANCED_FACE ( 'NONE', ( #6025 ), #4693, .T. ) ;
#9385 = CARTESIAN_POINT ( 'NONE',  ( -99.30949456653213758, -131.5229532012209290, 35.79133943910348847 ) ) ;
#9386 = CARTESIAN_POINT ( 'NONE',  ( 0.01899995639452935550, -7.352259170992699211, 5.265513565426384268 ) ) ;
#9387 = DIRECTION ( 'NONE',  ( -0.000000000000000000, -1.000000000000000000, -0.000000000000000000 ) ) ;
#9388 = DIRECTION ( 'NONE',  ( 1.000000000000000000, 0.000000000000000000, 0.000000000000000000 ) ) ;
#9389 = VERTEX_POINT ( 'NONE', #13986 ) ;
#9390 = CARTESIAN_POINT ( 'NONE',  ( -189.9999999999988916, 265.0000000000000000, 12.50000000000027178 ) ) ;
#9391 = LINE ( 'NONE', #6125, #7157 ) ;
#9392 = ORIENTED_EDGE ( 'NONE', *, *, #12737, .F. ) ;
#9393 = CARTESIAN_POINT ( 'NONE',  ( -78.17584345766714193, 126.7527627678825581, -19.23956518957315964 ) ) ;
#9394 = PLANE ( 'NONE',  #18260 ) ;
#9395 = DIRECTION ( 'NONE',  ( 1.000000000000000000, 0.000000000000000000, 0.000000000000000000 ) ) ;
#9396 = EDGE_CURVE ( 'NONE', #17652, #7267, #16968, .T. ) ;
#9397 = DIRECTION ( 'NONE',  ( 0.000000000000000000, 0.000000000000000000, 1.000000000000000000 ) ) ;
#9398 = DIRECTION ( 'NONE',  ( 1.000000000000000000, 0.000000000000000000, 0.000000000000000000 ) ) ;
#9399 = LINE ( 'NONE', #10612, #12494 ) ;
#9400 = ORIENTED_EDGE ( 'NONE', *, *, #20142, .T. ) ;
#9401 = PLANE ( 'NONE',  #15806 ) ;
#9402 = ORIENTED_EDGE ( 'NONE', *, *, #15277, .T. ) ;
#9403 = CIRCLE ( 'NONE', #8083, 77.50000000000000000 ) ;
#9404 = ORIENTED_EDGE ( 'NONE', *, *, #8667, .T. ) ;
#9405 = DIRECTION ( 'NONE',  ( 0.000000000000000000, 0.000000000000000000, 1.000000000000000000 ) ) ;
#9406 = AXIS2_PLACEMENT_3D ( 'NONE', #10536, #20165, #9323 ) ;
#9407 = ADVANCED_FACE ( 'NONE', ( #1413 ), #17278, .T. ) ;
#9408 = ORIENTED_EDGE ( 'NONE', *, *, #17186, .F. ) ;
#9409 = EDGE_CURVE ( 'NONE', #5147, #13667, #11079, .T. ) ;
#9410 = CARTESIAN_POINT ( 'NONE',  ( 17.50000000000001066, 0.000000000000000000, 83.57543755549745867 ) ) ;
#9411 = DIRECTION ( 'NONE',  ( 0.000000000000000000, 0.000000000000000000, 1.000000000000000000 ) ) ;
#9412 = ORIENTED_EDGE ( 'NONE', *, *, #16389, .T. ) ;
#9413 = CARTESIAN_POINT ( 'NONE',  ( 97.91442649640829643, -133.4097810207084081, 7.055758473159548849 ) ) ;
#9414 = DIRECTION ( 'NONE',  ( -0.000000000000000000, -0.000000000000000000, 1.000000000000000000 ) ) ;
#9415 = EDGE_CURVE ( 'NONE', #698, #599, #3569, .T. ) ;
#9416 = EDGE_CURVE ( 'NONE', #11180, #4182, #1622, .T. ) ;
#9417 = AXIS2_PLACEMENT_3D ( 'NONE', #3745, #2421, #578 ) ;
#9418 = DIRECTION ( 'NONE',  ( -0.000000000000000000, -0.000000000000000000, 1.000000000000000000 ) ) ;
#9419 = CIRCLE ( 'NONE', #11046, 7.500000000000007105 ) ;
#9420 = FILL_AREA_STYLE_COLOUR ( '', #3738 ) ;
#9421 = AXIS2_PLACEMENT_3D ( 'NONE', #13895, #1321, #13794 ) ;
#9422 = VERTEX_POINT ( 'NONE', #9288 ) ;
#9423 = FACE_OUTER_BOUND ( 'NONE', #4987, .T. ) ;
#9424 = CARTESIAN_POINT ( 'NONE',  ( -1.678175111358135130, -5.485913980968154746, 293.5832628385307999 ) ) ;
#9425 = LINE ( 'NONE', #12793, #2242 ) ;
#9426 = CARTESIAN_POINT ( 'NONE',  ( 87.54876440221090661, -121.8053786065073467, 44.23084021805906474 ) ) ;
#9427 = ORIENTED_EDGE ( 'NONE', *, *, #19467, .T. ) ;
#9428 = DIRECTION ( 'NONE',  ( 0.000000000000000000, 0.000000000000000000, 1.000000000000000000 ) ) ;
#9429 = CARTESIAN_POINT ( 'NONE',  ( -32.64570716507503079, 53.78543575132162857, 293.5832628385307999 ) ) ;
#9430 = EDGE_LOOP ( 'NONE', ( #7738, #697, #15597 ) ) ;
#9431 = VERTEX_POINT ( 'NONE', #3157 ) ;
#9432 = VERTEX_POINT ( 'NONE', #181 ) ;
#9433 = CARTESIAN_POINT ( 'NONE',  ( 0.000000000000000000, 0.000000000000000000, 0.000000000000000000 ) ) ;
#9434 = VECTOR ( 'NONE', #13364, 1000.000000000000114 ) ;
#9435 = CIRCLE ( 'NONE', #10389, 40.00000000000000711 ) ;
#9436 = ORIENTED_EDGE ( 'NONE', *, *, #19765, .T. ) ;
#9437 = VECTOR ( 'NONE', #13989, 1000.000000000000000 ) ;
#9438 = CARTESIAN_POINT ( 'NONE',  ( 126.5370453525553671, 80.55045718954890788, 39.99999999999999289 ) ) ;
#9439 = CIRCLE ( 'NONE', #1939, 60.74260934110282051 ) ;
#9440 = CARTESIAN_POINT ( 'NONE',  ( -13.12726406102078158, -59.30716253403180360, 283.5832628385307999 ) ) ;
#9441 = ORIENTED_EDGE ( 'NONE', *, *, #11091, .T. ) ;
#9442 = DIRECTION ( 'NONE',  ( 1.000000000000000000, 0.000000000000000000, 0.000000000000000000 ) ) ;
#9443 = CARTESIAN_POINT ( 'NONE',  ( -109.9999999999983515, 275.0000000000000000, 85.00000000000001421 ) ) ;
#9444 = EDGE_CURVE ( 'NONE', #19147, #6858, #79, .T. ) ;
#9445 = CARTESIAN_POINT ( 'NONE',  ( -101.4356266330729426, -128.4750511900866456, 37.97853139149559354 ) ) ;
#9446 = DIRECTION ( 'NONE',  ( 1.000000000000000000, 0.000000000000000000, -0.000000000000000000 ) ) ;
#9447 = CARTESIAN_POINT ( 'NONE',  ( -124.9072147131054180, 63.35168546091732367, 36.73018266758872130 ) ) ;
#9448 = DIRECTION ( 'NONE',  ( 0.000000000000000000, -0.000000000000000000, 1.000000000000000000 ) ) ;
#9449 = LINE ( 'NONE', #1776, #17059 ) ;
#9450 = VECTOR ( 'NONE', #10635, 1000.000000000000000 ) ;
#9451 = DIRECTION ( 'NONE',  ( -0.6427876096865300370, -0.7660444431189858960, 0.000000000000000000 ) ) ;
#9452 = LINE ( 'NONE', #8313, #2013 ) ;
#9453 = CIRCLE ( 'NONE', #938, 62.91752772691707207 ) ;
#9454 = CARTESIAN_POINT ( 'NONE',  ( -126.6625757374809638, -80.35588318643578987, 49.09314554429377608 ) ) ;
#9455 = AXIS2_PLACEMENT_3D ( 'NONE', #971, #15189, #13439 ) ;
#9456 = ORIENTED_EDGE ( 'NONE', *, *, #16313, .F. ) ;
#9457 = AXIS2_PLACEMENT_3D ( 'NONE', #13419, #11691, #7101 ) ;
#9458 = DIRECTION ( 'NONE',  ( 1.000000000000000000, 0.000000000000000000, -0.000000000000000000 ) ) ;
#9459 = ORIENTED_EDGE ( 'NONE', *, *, #1903, .F. ) ;
#9460 = ORIENTED_EDGE ( 'NONE', *, *, #7928, .F. ) ;
#9461 = ORIENTED_EDGE ( 'NONE', *, *, #8885, .F. ) ;
#9462 = CIRCLE ( 'NONE', #9781, 42.50000000000000000 ) ;
#9463 = AXIS2_PLACEMENT_3D ( 'NONE', #10989, #15291, #6098 ) ;
#9464 = EDGE_CURVE ( 'NONE', #7122, #13906, #7848, .T. ) ;
#9465 = DIRECTION ( 'NONE',  ( -0.8660254037844415942, 0.4999999999999949485, 0.000000000000000000 ) ) ;
#9466 = DIRECTION ( 'NONE',  ( 1.000000000000000000, 0.000000000000000000, 0.000000000000000000 ) ) ;
#9467 = CARTESIAN_POINT ( 'NONE',  ( 1.629865514042525776, 60.72073886220395877, 293.5832628385307999 ) ) ;
#9468 = VERTEX_POINT ( 'NONE', #15938 ) ;
#9469 = CYLINDRICAL_SURFACE ( 'NONE', #16623, 3.224098631618460331 ) ;
#9470 = CARTESIAN_POINT ( 'NONE',  ( 1.629865514042525554, 60.72073886220396588, 283.5832628385307999 ) ) ;
#9471 = CYLINDRICAL_SURFACE ( 'NONE', #1264, 112.8770930172170210 ) ;
#9472 = LINE ( 'NONE', #3232, #4598 ) ;
#9473 = CARTESIAN_POINT ( 'NONE',  ( -32.50000000000000000, 0.000000000000000000, -110.0000000000000000 ) ) ;
#9474 = EDGE_LOOP ( 'NONE', ( #13523, #6777, #18282, #2965 ) ) ;
#9475 = ADVANCED_FACE ( 'NONE', ( #14696 ), #485, .T. ) ;
#9476 = CARTESIAN_POINT ( 'NONE',  ( 133.2712073793125569, -68.96827650305596080, 29.99999999999999645 ) ) ;
#9477 = CARTESIAN_POINT ( 'NONE',  ( 131.2500704209023183, -90.93860529234677870, 39.99999999999998579 ) ) ;
#9478 = ORIENTED_EDGE ( 'NONE', *, *, #19156, .T. ) ;
#9479 = ORIENTED_EDGE ( 'NONE', *, *, #8714, .F. ) ;
#9480 = ORIENTED_EDGE ( 'NONE', *, *, #17738, .F. ) ;
#9481 = ORIENTED_EDGE ( 'NONE', *, *, #2790, .F. ) ;
#9482 = DIRECTION ( 'NONE',  ( -0.000000000000000000, -0.000000000000000000, 1.000000000000000000 ) ) ;
#9483 = PRODUCT_DEFINITION_SHAPE ( 'NONE', 'NONE',  #20244 ) ;
#9484 = VERTEX_POINT ( 'NONE', #11219 ) ;
#9485 = LINE ( 'NONE', #8044, #2187 ) ;
#9486 = ADVANCED_FACE ( 'NONE', ( #2326 ), #9790, .F. ) ;
#9487 = DIRECTION ( 'NONE',  ( -0.9009688679024207003, 0.4338837391175549563, 0.000000000000000000 ) ) ;
#9488 = DIRECTION ( 'NONE',  ( 0.9396926207859056523, -0.3420201433256757628, -6.584943678403441173E-15 ) ) ;
#9489 = AXIS2_PLACEMENT_3D ( 'NONE', #10716, #6034, #1006 ) ;
#9490 = CARTESIAN_POINT ( 'NONE',  ( 57.92514141135451666, 18.28503710798567994, 283.5832628385307999 ) ) ;
#9491 = DIRECTION ( 'NONE',  ( 0.9396926207859063185, -0.3420201433256742640, -6.456589605409180904E-15 ) ) ;
#9492 = ORIENTED_EDGE ( 'NONE', *, *, #17547, .T. ) ;
#9493 = AXIS2_PLACEMENT_3D ( 'NONE', #1955, #17309, #14330 ) ;
#9494 = CARTESIAN_POINT ( 'NONE',  ( -141.8714406926360994, -48.70825716237271763, 49.99999999999999289 ) ) ;
#9495 = CARTESIAN_POINT ( 'NONE',  ( -110.0000000000000142, 265.0000000000000000, 5.000000000000000888 ) ) ;
#9496 = ORIENTED_EDGE ( 'NONE', *, *, #2535, .F. ) ;
#9497 = CARTESIAN_POINT ( 'NONE',  ( -110.0000000000000000, 88.56916956954178488, -34.99999999999998579 ) ) ;
#9498 = DIRECTION ( 'NONE',  ( -0.000000000000000000, -1.000000000000000000, -0.000000000000000000 ) ) ;
#9499 = CARTESIAN_POINT ( 'NONE',  ( 18.28567271940513450, -57.92709869106715814, 293.5832628385307999 ) ) ;
#9500 = CARTESIAN_POINT ( 'NONE',  ( -52.50000000000000000, -2.094888803305880013E-13, -105.0000000000000142 ) ) ;
#9501 = EDGE_CURVE ( 'NONE', #18959, #4038, #13145, .T. ) ;
#9502 = CARTESIAN_POINT ( 'NONE',  ( 0.000000000000000000, 0.000000000000000000, 248.9926560891072143 ) ) ;
#9503 = CARTESIAN_POINT ( 'NONE',  ( 98.63291732527038391, -113.0135401039851217, 49.87660771364959089 ) ) ;
#9504 = EDGE_LOOP ( 'NONE', ( #2337, #12892, #9404, #19733, #14105 ) ) ;
#9505 = EDGE_CURVE ( 'NONE', #12416, #8371, #10105, .T. ) ;
#9506 = CIRCLE ( 'NONE', #14412, 3.224098631618461663 ) ;
#9507 = DIRECTION ( 'NONE',  ( 1.000000000000000000, 0.000000000000000000, 0.000000000000000000 ) ) ;
#9508 = VERTEX_POINT ( 'NONE', #19018 ) ;
#9509 = AXIS2_PLACEMENT_3D ( 'NONE', #9818, #16471, #5322 ) ;
#9510 = ORIENTED_EDGE ( 'NONE', *, *, #9102, .F. ) ;
#9511 = DIRECTION ( 'NONE',  ( -0.9271237148521536131, 0.3747554100459959958, 0.000000000000000000 ) ) ;
#9512 = ORIENTED_EDGE ( 'NONE', *, *, #9267, .T. ) ;
#9513 = DIRECTION ( 'NONE',  ( 0.000000000000000000, 0.000000000000000000, -1.000000000000000000 ) ) ;
#9514 = EDGE_CURVE ( 'NONE', #14876, #1151, #9991, .T. ) ;
#9515 = LINE ( 'NONE', #12974, #5348 ) ;
#9516 = EDGE_LOOP ( 'NONE', ( #18737, #15826, #2236 ) ) ;
#9517 = CARTESIAN_POINT ( 'NONE',  ( 0.000000000000000000, -7.794228634059948035, -4.499999999999999112 ) ) ;
#9518 = DIRECTION ( 'NONE',  ( 1.000000000000000000, 0.000000000000000000, 0.000000000000000000 ) ) ;
#9519 = VECTOR ( 'NONE', #512, 1000.000000000000000 ) ;
#9520 = VECTOR ( 'NONE', #18768, 1000.000000000000000 ) ;
#9521 = DIRECTION ( 'NONE',  ( -0.5300553768524346454, -0.8479630283625717579, 0.000000000000000000 ) ) ;
#9522 = CARTESIAN_POINT ( 'NONE',  ( -5.524863963826822655, -116.0870680293436408, 14.88498244535549020 ) ) ;
#9523 = EDGE_LOOP ( 'NONE', ( #14711, #6250, #10318, #8442 ) ) ;
#9524 = CYLINDRICAL_SURFACE ( 'NONE', #19677, 60.74260934110282051 ) ;
#9525 = DIRECTION ( 'NONE',  ( 1.000000000000000000, 0.000000000000000000, -0.000000000000000000 ) ) ;
#9526 = EDGE_CURVE ( 'NONE', #12122, #18228, #18592, .T. ) ;
#9527 = CARTESIAN_POINT ( 'NONE',  ( 152.4599531637113330, -36.50981547336952104, 39.99999999999999289 ) ) ;
#9528 = CARTESIAN_POINT ( 'NONE',  ( 85.14104117559514862, -123.4951580371803885, 41.03646238235858590 ) ) ;
#9529 = ORIENTED_EDGE ( 'NONE', *, *, #18154, .F. ) ;
#9530 = EDGE_CURVE ( 'NONE', #10395, #8936, #5393, .T. ) ;
#9531 = EDGE_CURVE ( 'NONE', #17394, #8237, #1926, .T. ) ;
#9532 = CARTESIAN_POINT ( 'NONE',  ( -97.95177330934026827, 59.60912842347561025, 14.88498244535613502 ) ) ;
#9533 = CARTESIAN_POINT ( 'NONE',  ( -92.96950599336983601, 117.7174478370289279, 41.20115630078900182 ) ) ;
#9534 = VERTEX_POINT ( 'NONE', #6928 ) ;
#9535 = EDGE_LOOP ( 'NONE', ( #3277, #6142, #4079, #5168 ) ) ;
#9536 = ORIENTED_EDGE ( 'NONE', *, *, #12400, .T. ) ;
#9537 = DIRECTION ( 'NONE',  ( 0.000000000000000000, 0.000000000000000000, 1.000000000000000000 ) ) ;
#9538 = VERTEX_POINT ( 'NONE', #19409 ) ;
#9539 = LINE ( 'NONE', #26, #11722 ) ;
#9540 = CARTESIAN_POINT ( 'NONE',  ( -1.396592535537253342E-14, 0.000000000000000000, 39.88498244535545467 ) ) ;
#9541 = EDGE_CURVE ( 'NONE', #16770, #16122, #3846, .T. ) ;
#9542 = ORIENTED_EDGE ( 'NONE', *, *, #18534, .T. ) ;
#9543 = CARTESIAN_POINT ( 'NONE',  ( -77.31114765718484705, 12.23146955673673197, 112.0427633081292385 ) ) ;
#9544 = CARTESIAN_POINT ( 'NONE',  ( 141.8714406926368099, -48.70825716237082759, 49.99999999999999289 ) ) ;
#9545 = CARTESIAN_POINT ( 'NONE',  ( 130.1925331961320182, -74.50863253846080170, 46.29641651522450729 ) ) ;
#9546 = CARTESIAN_POINT ( 'NONE',  ( -84.61443574189109995, -123.8565353992701858, 40.13652017786752424 ) ) ;
#9547 = CARTESIAN_POINT ( 'NONE',  ( -17.49999999999999289, 2.143131898507871009E-15, 49.99999999999998579 ) ) ;
#9548 = DIRECTION ( 'NONE',  ( 1.000000000000000000, 0.000000000000000000, 0.000000000000000000 ) ) ;
#9549 = CARTESIAN_POINT ( 'NONE',  ( 1.396592535537253342E-14, 0.000000000000000000, 49.99999999999999289 ) ) ;
#9550 = LINE ( 'NONE', #443, #14449 ) ;
#9551 = EDGE_CURVE ( 'NONE', #3116, #1080, #8352, .T. ) ;
#9552 = DIRECTION ( 'NONE',  ( 0.9848077530122080203, 0.1736481776669306920, 0.000000000000000000 ) ) ;
#9553 = FACE_OUTER_BOUND ( 'NONE', #9703, .T. ) ;
#9554 = CARTESIAN_POINT ( 'NONE',  ( -131.8028587768753823, -71.61967917966801167, 44.00945860701838086 ) ) ;
#9555 = ORIENTED_EDGE ( 'NONE', *, *, #14758, .T. ) ;
#9556 = CARTESIAN_POINT ( 'NONE',  ( 67.50000000000000000, 6.284666409917639535E-13, -100.0000000000000000 ) ) ;
#9557 = VECTOR ( 'NONE', #7503, 1000.000000000000000 ) ;
#9558 = AXIS2_PLACEMENT_3D ( 'NONE', #15814, #9769, #18994 ) ;
#9559 = EDGE_CURVE ( 'NONE', #6626, #18719, #581, .T. ) ;
#9560 = EDGE_LOOP ( 'NONE', ( #12202, #12543, #17670 ) ) ;
#9561 = CIRCLE ( 'NONE', #12153, 62.91752772691707207 ) ;
#9562 = VERTEX_POINT ( 'NONE', #13053 ) ;
#9563 = ORIENTED_EDGE ( 'NONE', *, *, #360, .T. ) ;
#9564 = CARTESIAN_POINT ( 'NONE',  ( -142.4959821499880945, -17.39774326699847151, -8.008195377800351622 ) ) ;
#9565 = CARTESIAN_POINT ( 'NONE',  ( 0.8220851292435327196, 78.26059000578311498, 112.7772637782949943 ) ) ;
#9566 = DIRECTION ( 'NONE',  ( 1.000000000000000000, 0.000000000000000000, 0.000000000000000000 ) ) ;
#9567 = AXIS2_PLACEMENT_3D ( 'NONE', #15971, #11151, #6360 ) ;
#9568 = CARTESIAN_POINT ( 'NONE',  ( 0.000000000000000000, 1.102182119232617911E-15, -9.000000000000001776 ) ) ;
#9569 = CARTESIAN_POINT ( 'NONE',  ( 54.89456854707540856, 30.74413178637211885, 293.5832628385307999 ) ) ;
#9570 = CARTESIAN_POINT ( 'NONE',  ( 81.66698895276897474, 79.37254397626031732, 39.88498244535488624 ) ) ;
#9571 = CARTESIAN_POINT ( 'NONE',  ( 0.000000000000000000, 0.000000000000000000, 49.99999999999999289 ) ) ;
#9572 = AXIS2_PLACEMENT_3D ( 'NONE', #8590, #14828, #17911 ) ;
#9573 = CARTESIAN_POINT ( 'NONE',  ( 0.000000000000000000, 0.000000000000000000, 49.99999999999999289 ) ) ;
#9574 = CYLINDRICAL_SURFACE ( 'NONE', #10054, 60.74260934110282051 ) ;
#9575 = VERTEX_POINT ( 'NONE', #14401 ) ;
#9576 = CARTESIAN_POINT ( 'NONE',  ( 134.6268015237237705, -73.65543454550100932, 32.58577753858380532 ) ) ;
#9577 = CARTESIAN_POINT ( 'NONE',  ( 134.2328839869800845, -76.48032294689464550, 35.58107860435188741 ) ) ;
#9578 = VERTEX_POINT ( 'NONE', #382 ) ;
#9579 = CIRCLE ( 'NONE', #3361, 60.74260934110282051 ) ;
#9580 = VECTOR ( 'NONE', #15783, 1000.000000000000000 ) ;
#9581 = ORIENTED_EDGE ( 'NONE', *, *, #7286, .T. ) ;
#9582 = ORIENTED_EDGE ( 'NONE', *, *, #16197, .F. ) ;
#9583 = LINE ( 'NONE', #3248, #11540 ) ;
#9584 = ORIENTED_EDGE ( 'NONE', *, *, #19859, .T. ) ;
#9585 = DIRECTION ( 'NONE',  ( 0.9848077530122080203, 0.1736481776669306920, 0.000000000000000000 ) ) ;
#9586 = VECTOR ( 'NONE', #13256, 1000.000000000000114 ) ;
#9587 = CARTESIAN_POINT ( 'NONE',  ( -97.49999999999998579, -133.9542832461881687, 30.00000000000000000 ) ) ;
#9588 = DIRECTION ( 'NONE',  ( 0.000000000000000000, 1.000000000000000000, 0.000000000000000000 ) ) ;
#9589 = CARTESIAN_POINT ( 'NONE',  ( 26.85905058935142975, 1.464553941565464035, 14.88498244535526460 ) ) ;
#9590 = ORIENTED_EDGE ( 'NONE', *, *, #18361, .T. ) ;
#9591 = DIRECTION ( 'NONE',  ( 1.000000000000000000, 0.000000000000000000, 0.000000000000000000 ) ) ;
#9592 = CARTESIAN_POINT ( 'NONE',  ( -3.391519920806218558E-15, 7.351593252548065394, 5.266666970006217419 ) ) ;
#9593 = ORIENTED_EDGE ( 'NONE', *, *, #18942, .T. ) ;
#9594 = DIRECTION ( 'NONE',  ( 0.6427876096865353661, 0.7660444431189813441, 0.000000000000000000 ) ) ;
#9596 = CIRCLE ( 'NONE', #5663, 60.74260934110282051 ) ;
#9595 = CARTESIAN_POINT ( 'NONE',  ( 30.53958573130908505, -50.13752642112839197, 110.9660488491356887 ) ) ;
#9597 = DIRECTION ( 'NONE',  ( -0.000000000000000000, -0.000000000000000000, 1.000000000000000000 ) ) ;
#9598 = DIRECTION ( 'NONE',  ( -0.1736481776669409338, -0.9848077530122062440, 1.076098267568195634E-15 ) ) ;
#9599 = CARTESIAN_POINT ( 'NONE',  ( -20.01059462374426445, -13.41455640552162443, 14.88498244535559323 ) ) ;
#9600 = VECTOR ( 'NONE', #13746, 1000.000000000000000 ) ;
#9601 = CARTESIAN_POINT ( 'NONE',  ( 82.53664710575304753, -125.2505858294166501, 34.62610835550965049 ) ) ;
#9602 = VERTEX_POINT ( 'NONE', #684 ) ;
#9603 = EDGE_CURVE ( 'NONE', #8683, #6975, #16339, .T. ) ;
#9604 = DIRECTION ( 'NONE',  ( 1.000000000000000000, 0.000000000000000000, 0.000000000000000000 ) ) ;
#9605 = ORIENTED_EDGE ( 'NONE', *, *, #14143, .F. ) ;
#9606 = ORIENTED_EDGE ( 'NONE', *, *, #3460, .F. ) ;
#9607 = CARTESIAN_POINT ( 'NONE',  ( 25.99419088092191643, -73.82206860051540787, 132.4711112102474146 ) ) ;
#9608 = ORIENTED_EDGE ( 'NONE', *, *, #174, .T. ) ;
#9609 = CARTESIAN_POINT ( 'NONE',  ( -140.7359356944403430, 47.72516008681479605, -20.67287135512269813 ) ) ;
#9610 = EDGE_CURVE ( 'NONE', #8547, #15546, #18944, .T. ) ;
#9611 = LINE ( 'NONE', #18940, #4366 ) ;
#9612 = VERTEX_POINT ( 'NONE', #3749 ) ;
#9613 = EDGE_CURVE ( 'NONE', #5657, #2071, #14500, .T. ) ;
#9614 =( NAMED_UNIT ( * ) SI_UNIT ( $, .STERADIAN. ) SOLID_ANGLE_UNIT ( ) );
#9615 = DIRECTION ( 'NONE',  ( 0.9396926207859114255, -0.3420201433256601642, 0.000000000000000000 ) ) ;
#9616 = EDGE_CURVE ( 'NONE', #6558, #11573, #18262, .T. ) ;
#9617 = CYLINDRICAL_SURFACE ( 'NONE', #17370, 7.500000000000020428 ) ;
#9618 = AXIS2_PLACEMENT_3D ( 'NONE', #18883, #3221, #12623 ) ;
#9619 = CYLINDRICAL_SURFACE ( 'NONE', #18323, 106.4288957539801004 ) ;
#9620 = CARTESIAN_POINT ( 'NONE',  ( 14.94814811854963388, -76.83212392882496999, 248.9926560891072143 ) ) ;
#9621 = ORIENTED_EDGE ( 'NONE', *, *, #10622, .F. ) ;
#9622 = CARTESIAN_POINT ( 'NONE',  ( 0.000000000000000000, 0.000000000000000000, 293.5832628385307999 ) ) ;
#9623 = CARTESIAN_POINT ( 'NONE',  ( -79.75827554147308263, 9.767571684737763671E-15, 248.9926560891072143 ) ) ;
#9624 = DIRECTION ( 'NONE',  ( 0.9993852124581887875, -0.03505990758545544927, 0.000000000000000000 ) ) ;
#9625 = CARTESIAN_POINT ( 'NONE',  ( -110.0000000000000142, 275.0000000000000568, -29.99999999999998224 ) ) ;
#9626 = EDGE_LOOP ( 'NONE', ( #7457, #5430, #15077, #3240 ) ) ;
#9627 = EDGE_CURVE ( 'NONE', #17740, #4738, #11327, .T. ) ;
#9628 = DIRECTION ( 'NONE',  ( -0.6155349844899689060, 0.7881095627315620744, 0.000000000000000000 ) ) ;
#9629 = CARTESIAN_POINT ( 'NONE',  ( -70.58469675536078114, 132.3548539117337270, 11.82943511394700487 ) ) ;
#9630 = ORIENTED_EDGE ( 'NONE', *, *, #14641, .F. ) ;
#9631 = PRESENTATION_LAYER_ASSIGNMENT (  '', '', ( #19433 ) ) ;
#9632 = EDGE_LOOP ( 'NONE', ( #1331, #4162, #7417, #15373 ) ) ;
#9633 = EDGE_LOOP ( 'NONE', ( #15613, #18021 ) ) ;
#9634 = SHAPE_DEFINITION_REPRESENTATION ( #10940, #16185 ) ;
#9635 = ORIENTED_EDGE ( 'NONE', *, *, #11168, .F. ) ;
#9636 = CARTESIAN_POINT ( 'NONE',  ( -100.6828170698202172, -129.5784119885790915, 2.652022552455725268 ) ) ;
#9637 = CARTESIAN_POINT ( 'NONE',  ( -149.9875400927184046, 2.232080205859953370, 6.152641185304041471 ) ) ;
#9638 = ORIENTED_EDGE ( 'NONE', *, *, #1138, .T. ) ;
#9639 = ADVANCED_FACE ( 'NONE', ( #14990 ), #11906, .T. ) ;
#9640 = AXIS2_PLACEMENT_3D ( 'NONE', #8870, #10601, #7340 ) ;
#9641 = CARTESIAN_POINT ( 'NONE',  ( 0.8038475772933695307, 10.39230484541327471, -5.094467845664485666E-17 ) ) ;
#9642 = CARTESIAN_POINT ( 'NONE',  ( 131.9010376021428783, -71.43117396976204247, 43.79329771262451487 ) ) ;
#9643 = EDGE_CURVE ( 'NONE', #8342, #7122, #6526, .T. ) ;
#9644 = CARTESIAN_POINT ( 'NONE',  ( -120.6301673961016547, 71.05871668019251786, 38.35088066313576149 ) ) ;
#9645 = FACE_OUTER_BOUND ( 'NONE', #4811, .T. ) ;
#9646 = DIRECTION ( 'NONE',  ( -0.000000000000000000, -0.000000000000000000, 1.000000000000000000 ) ) ;
#9647 = FACE_OUTER_BOUND ( 'NONE', #864, .T. ) ;
#9648 = DIRECTION ( 'NONE',  ( 1.000000000000000000, 0.000000000000000000, -6.994638739193275171E-15 ) ) ;
#9649 = CYLINDRICAL_SURFACE ( 'NONE', #6715, 42.50000000000000000 ) ;
#9650 = ORIENTED_EDGE ( 'NONE', *, *, #4242, .T. ) ;
#9651 = EDGE_CURVE ( 'NONE', #10444, #937, #6193, .T. ) ;
#9652 = PRODUCT ( 'Base Flange', 'Base Flange', '', ( #8197 ) ) ;
#9653 = DIRECTION ( 'NONE',  ( -0.000000000000000000, -0.000000000000000000, 1.000000000000000000 ) ) ;
#9654 = CIRCLE ( 'NONE', #11272, 10.00000000000000888 ) ;
#9655 = ORIENTED_EDGE ( 'NONE', *, *, #7511, .F. ) ;
#9656 = EDGE_LOOP ( 'NONE', ( #4442, #7763, #16062, #19098 ) ) ;
#9657 = ADVANCED_FACE ( 'NONE', ( #19502 ), #17629, .T. ) ;
#9659 = EDGE_CURVE ( 'NONE', #19327, #13999, #10283, .T. ) ;
#9658 = CONICAL_SURFACE ( 'NONE', #9981, 32.50000000000000000, 0.7853981633974510546 ) ;
#9660 = EDGE_CURVE ( 'NONE', #1187, #15465, #7812, .T. ) ;
#9661 = CARTESIAN_POINT ( 'NONE',  ( 0.000000000000000000, 0.000000000000000000, -115.0000000000000000 ) ) ;
#9662 = CARTESIAN_POINT ( 'NONE',  ( -176.1792632384392050, -186.5724904703759535, 40.00000000000000000 ) ) ;
#9664 = CARTESIAN_POINT ( 'NONE',  ( 1.629865514042525776, 60.72073886220395877, 283.5832628385307999 ) ) ;
#9663 = CIRCLE ( 'NONE', #12268, 62.91752772691707207 ) ;
#9665 = LINE ( 'NONE', #9568, #4225 ) ;
#9666 = ADVANCED_FACE ( 'NONE', ( #7415 ), #16442, .F. ) ;
#9667 = DIRECTION ( 'NONE',  ( -0.000000000000000000, -0.000000000000000000, 1.000000000000000000 ) ) ;
#9668 = DIRECTION ( 'NONE',  ( -6.982962677686266711E-15, 0.000000000000000000, -1.000000000000000000 ) ) ;
#9669 = DIRECTION ( 'NONE',  ( 1.000000000000000000, 1.047444401652940164E-14, 0.000000000000000000 ) ) ;
#9670 = EDGE_CURVE ( 'NONE', #15465, #9091, #2425, .T. ) ;
#9671 = CARTESIAN_POINT ( 'NONE',  ( 100.6828170698202314, -129.5784119885790346, 37.34797744754428095 ) ) ;
#9672 = DIRECTION ( 'NONE',  ( 0.000000000000000000, 0.000000000000000000, -1.000000000000000000 ) ) ;
#9673 = ORIENTED_EDGE ( 'NONE', *, *, #13333, .F. ) ;
#9674 = CARTESIAN_POINT ( 'NONE',  ( 129.7881937802467860, -75.28665481069999998, 39.48948438905874525 ) ) ;
#9675 = CARTESIAN_POINT ( 'NONE',  ( 133.8332678793154287, -78.98710468785299099, 37.05447038645785085 ) ) ;
#9676 = VECTOR ( 'NONE', #11551, 1000.000000000000000 ) ;
#9677 = EDGE_LOOP ( 'NONE', ( #9354, #3325 ) ) ;
#9678 = ORIENTED_EDGE ( 'NONE', *, *, #8365, .T. ) ;
#9679 = ORIENTED_EDGE ( 'NONE', *, *, #12607, .T. ) ;
#9680 = DIRECTION ( 'NONE',  ( -0.000000000000000000, -0.000000000000000000, 1.000000000000000000 ) ) ;
#9681 = VECTOR ( 'NONE', #8235, 1000.000000000000000 ) ;
#9682 = ORIENTED_EDGE ( 'NONE', *, *, #6449, .F. ) ;
#9683 = CARTESIAN_POINT ( 'NONE',  ( -13.12769224524071277, -59.30917539369501412, 293.5832628385307999 ) ) ;
#9684 = CARTESIAN_POINT ( 'NONE',  ( -36.71940246244727035, 108.6254278180370250, 39.88498244535571047 ) ) ;
#9685 = DIRECTION ( 'NONE',  ( -0.6692498792541777819, -0.7430374143461878633, 0.000000000000000000 ) ) ;
#9686 = CARTESIAN_POINT ( 'NONE',  ( 57.94128254008182921, 9.381844291199925578, 112.0427633081291816 ) ) ;
#9687 = ORIENTED_EDGE ( 'NONE', *, *, #11828, .F. ) ;
#9688 = DIRECTION ( 'NONE',  ( 1.000000000000000000, 0.000000000000000000, 0.000000000000000000 ) ) ;
#9689 = CARTESIAN_POINT ( 'NONE',  ( -27.10287801637868199, 1.507547295587424951, 14.88498244535564297 ) ) ;
#9690 = VECTOR ( 'NONE', #9291, 1000.000000000000000 ) ;
#9691 = VERTEX_POINT ( 'NONE', #8746 ) ;
#9692 = DIRECTION ( 'NONE',  ( 1.000000000000000000, 0.000000000000000000, 0.000000000000000000 ) ) ;
#9693 = DIRECTION ( 'NONE',  ( -0.000000000000000000, -0.000000000000000000, -1.000000000000000000 ) ) ;
#9694 = CARTESIAN_POINT ( 'NONE',  ( -71.18887634719365565, -147.8252249328922687, 39.99999999999999289 ) ) ;
#9695 = DIRECTION ( 'NONE',  ( -0.000000000000000000, -0.000000000000000000, 1.000000000000000000 ) ) ;
#9696 = AXIS2_PLACEMENT_3D ( 'NONE', #16374, #19341, #17713 ) ;
#9697 = FACE_OUTER_BOUND ( 'NONE', #16842, .T. ) ;
#9698 = CYLINDRICAL_SURFACE ( 'NONE', #14709, 150.0000000000000284 ) ;
#9699 = CARTESIAN_POINT ( 'NONE',  ( 82.79607015190580910, -125.0792639210692982, 35.66528578544987482 ) ) ;
#9700 = ORIENTED_EDGE ( 'NONE', *, *, #16281, .F. ) ;
#9701 = PLANE ( 'NONE',  #3061 ) ;
#9702 = ORIENTED_EDGE ( 'NONE', *, *, #17917, .T. ) ;
#9703 = EDGE_LOOP ( 'NONE', ( #1078, #5691, #18250, #16383 ) ) ;
#9704 = CARTESIAN_POINT ( 'NONE',  ( 22.28973221005081484, 58.83691981461641518, 248.9926560891072143 ) ) ;
#9705 = VERTEX_POINT ( 'NONE', #19594 ) ;
#9706 = DIRECTION ( 'NONE',  ( 6.982962677686266711E-15, 0.000000000000000000, 1.000000000000000000 ) ) ;
#9707 = VECTOR ( 'NONE', #4178, 1000.000000000000114 ) ;
#9708 = DIRECTION ( 'NONE',  ( 6.982962677686266711E-15, -0.000000000000000000, 1.000000000000000000 ) ) ;
#9709 = EDGE_LOOP ( 'NONE', ( #2075, #16929, #4597, #16947 ) ) ;
#9710 = CARTESIAN_POINT ( 'NONE',  ( -163.5019688434124419, -20.99123081650240863, 60.00000000000000000 ) ) ;
#9711 = EDGE_CURVE ( 'NONE', #6026, #14067, #7480, .T. ) ;
#9712 = CARTESIAN_POINT ( 'NONE',  ( 0.000000000000000000, 0.000000000000000000, 6.000000000000001776 ) ) ;
#9713 = CARTESIAN_POINT ( 'NONE',  ( 101.0196388379316659, 100.9199429146863167, 39.99999999999999289 ) ) ;
#9714 = LINE ( 'NONE', #4931, #13396 ) ;
#9715 = DIRECTION ( 'NONE',  ( 0.000000000000000000, 0.000000000000000000, -1.000000000000000000 ) ) ;
#9716 = ORIENTED_EDGE ( 'NONE', *, *, #764, .F. ) ;
#9717 = CARTESIAN_POINT ( 'NONE',  ( -17.49999999999999289, 0.000000000000000000, 60.00000000000000000 ) ) ;
#9718 = DIRECTION ( 'NONE',  ( 0.000000000000000000, 0.000000000000000000, 1.000000000000000000 ) ) ;
#9719 = CARTESIAN_POINT ( 'NONE',  ( 159.9599531637113330, -36.50981547336952104, 49.99999999999999289 ) ) ;
#9720 = DIRECTION ( 'NONE',  ( 0.9848077530122085754, -0.1736481776669273336, 0.000000000000000000 ) ) ;
#9721 = AXIS2_PLACEMENT_3D ( 'NONE', #10090, #8349, #16336 ) ;
#9722 = VERTEX_POINT ( 'NONE', #17977 ) ;
#9723 = AXIS2_PLACEMENT_3D ( 'NONE', #14607, #5401, #6835 ) ;
#9724 = EDGE_CURVE ( 'NONE', #18854, #10141, #1609, .T. ) ;
#9725 = DIRECTION ( 'NONE',  ( 0.000000000000000000, 0.000000000000000000, -1.000000000000000000 ) ) ;
#9726 = CARTESIAN_POINT ( 'NONE',  ( 0.000000000000000000, 0.000000000000000000, -115.0000000000000000 ) ) ;
#9727 = AXIS2_PLACEMENT_3D ( 'NONE', #2605, #10455, #14968 ) ;
#9728 = EDGE_LOOP ( 'NONE', ( #4049, #18983 ) ) ;
#9729 = ORIENTED_EDGE ( 'NONE', *, *, #4787, .F. ) ;
#9730 = ADVANCED_FACE ( 'NONE', ( #10373 ), #20237, .T. ) ;
#9731 = VERTEX_POINT ( 'NONE', #873 ) ;
#9732 = ORIENTED_EDGE ( 'NONE', *, *, #5285, .T. ) ;
#9733 = CARTESIAN_POINT ( 'NONE',  ( -126.6376994899158177, 80.42828178209725820, 41.40291032811695970 ) ) ;
#9734 = ORIENTED_EDGE ( 'NONE', *, *, #1218, .T. ) ;
#9735 = CARTESIAN_POINT ( 'NONE',  ( 44.89578954330581695, 107.1965464310834477, 14.88498244535514026 ) ) ;
#9736 = PLANE ( 'NONE',  #12539 ) ;
#9737 = CARTESIAN_POINT ( 'NONE',  ( 0.000000000000000000, 0.000000000000000000, 0.000000000000000000 ) ) ;
#9738 = VECTOR ( 'NONE', #15394, 1000.000000000000114 ) ;
#9739 = EDGE_CURVE ( 'NONE', #7332, #5360, #9130, .T. ) ;
#9740 = AXIS2_PLACEMENT_3D ( 'NONE', #691, #6934, #13153 ) ;
#9741 = DIRECTION ( 'NONE',  ( 6.982962677686266711E-15, -0.000000000000000000, 1.000000000000000000 ) ) ;
#9742 = DIRECTION ( 'NONE',  ( 1.000000000000000000, 0.000000000000000000, -6.994638739193269649E-15 ) ) ;
#9743 = DIRECTION ( 'NONE',  ( -0.000000000000000000, -0.000000000000000000, 1.000000000000000000 ) ) ;
#9744 = DIRECTION ( 'NONE',  ( 0.000000000000000000, 0.000000000000000000, 1.000000000000000000 ) ) ;
#9745 = DIRECTION ( 'NONE',  ( 0.000000000000000000, 0.000000000000000000, -1.000000000000000000 ) ) ;
#9746 = FACE_OUTER_BOUND ( 'NONE', #1911, .T. ) ;
#9747 = DIRECTION ( 'NONE',  ( -0.000000000000000000, -0.000000000000000000, 1.000000000000000000 ) ) ;
#9748 = ORIENTED_EDGE ( 'NONE', *, *, #1015, .T. ) ;
#9749 = EDGE_CURVE ( 'NONE', #5784, #16453, #5549, .T. ) ;
#9750 = DIRECTION ( 'NONE',  ( 0.9396926207859068736, 0.3420201433256726542, -0.000000000000000000 ) ) ;
#9751 = CIRCLE ( 'NONE', #1966, 10.00000000000000888 ) ;
#9752 = EDGE_CURVE ( 'NONE', #15281, #6318, #11421, .T. ) ;
#9753 = AXIS2_PLACEMENT_3D ( 'NONE', #18830, #19035, #7765 ) ;
#9754 = AXIS2_PLACEMENT_3D ( 'NONE', #7546, #18095, #18299 ) ;
#9755 = VECTOR ( 'NONE', #526, 1000.000000000000000 ) ;
#9756 = ORIENTED_EDGE ( 'NONE', *, *, #19291, .T. ) ;
#9757 = ORIENTED_EDGE ( 'NONE', *, *, #15009, .T. ) ;
#9758 = VERTEX_POINT ( 'NONE', #18267 ) ;
#9759 = CARTESIAN_POINT ( 'NONE',  ( 167.4599531637113330, -36.50981547336952104, 39.99999999999999289 ) ) ;
#9760 = EDGE_CURVE ( 'NONE', #2667, #5578, #15001, .T. ) ;
#9761 = CARTESIAN_POINT ( 'NONE',  ( -1.379293853801755176, 62.91752772691707207, 248.9926560891072143 ) ) ;
#9762 = CARTESIAN_POINT ( 'NONE',  ( 0.000000000000000000, 0.000000000000000000, 293.5832628385307999 ) ) ;
#9763 = LINE ( 'NONE', #14673, #6850 ) ;
#9764 = AXIS2_PLACEMENT_3D ( 'NONE', #977, #15609, #1597 ) ;
#9765 = AXIS2_PLACEMENT_3D ( 'NONE', #15085, #14887, #13343 ) ;
#9766 = EDGE_CURVE ( 'NONE', #19640, #12693, #10475, .T. ) ;
#9767 = DIRECTION ( 'NONE',  ( -0.000000000000000000, 0.000000000000000000, -1.000000000000000000 ) ) ;
#9768 = AXIS2_PLACEMENT_3D ( 'NONE', #18201, #4185, #18072 ) ;
#9769 = DIRECTION ( 'NONE',  ( 0.000000000000000000, 0.000000000000000000, 1.000000000000000000 ) ) ;
#9770 = PLANE ( 'NONE',  #6201 ) ;
#9771 = CARTESIAN_POINT ( 'NONE',  ( 101.1753893487742175, -128.8598102521083604, 37.76972961429584075 ) ) ;
#9772 = LINE ( 'NONE', #19194, #16910 ) ;
#9773 = ORIENTED_EDGE ( 'NONE', *, *, #16163, .F. ) ;
#9774 = EDGE_CURVE ( 'NONE', #14265, #5572, #12111, .T. ) ;
#9775 = ADVANCED_FACE ( 'NONE', ( #14794 ), #779, .F. ) ;
#9776 = CARTESIAN_POINT ( 'NONE',  ( 60.72279549541555355, -1.629937663769388090, 283.5832628385307999 ) ) ;
#9777 = ORIENTED_EDGE ( 'NONE', *, *, #12340, .T. ) ;
#9778 = CIRCLE ( 'NONE', #4550, 112.8770930172170068 ) ;
#9779 = EDGE_LOOP ( 'NONE', ( #11617, #9773, #5264, #16326 ) ) ;
#9780 = ORIENTED_EDGE ( 'NONE', *, *, #4212, .T. ) ;
#9781 = AXIS2_PLACEMENT_3D ( 'NONE', #18963, #14242, #4948 ) ;
#9782 = ORIENTED_EDGE ( 'NONE', *, *, #1273, .F. ) ;
#9783 = ORIENTED_EDGE ( 'NONE', *, *, #7240, .F. ) ;
#9784 = CARTESIAN_POINT ( 'NONE',  ( 159.9599531637113330, -36.50981547336952104, 39.99999999999999289 ) ) ;
#9785 = CARTESIAN_POINT ( 'NONE',  ( -98.51475352695842957, -132.6070668284233136, 34.40940853324102733 ) ) ;
#9786 = CARTESIAN_POINT ( 'NONE',  ( 0.2993243175132176415, -5.729042578294388122, 293.5832628385307999 ) ) ;
#9787 = CARTESIAN_POINT ( 'NONE',  ( -110.0000000000000142, 285.0000000000000568, -94.99999999999997158 ) ) ;
#9788 = ORIENTED_EDGE ( 'NONE', *, *, #12837, .F. ) ;
#9789 = DIRECTION ( 'NONE',  ( 0.000000000000000000, 0.000000000000000000, 1.000000000000000000 ) ) ;
#9790 = PLANE ( 'NONE',  #14364 ) ;
#9791 = VERTEX_POINT ( 'NONE', #1691 ) ;
#9792 = CARTESIAN_POINT ( 'NONE',  ( -99.16663380741609046, 102.1467062937776120, -33.51457741426627734 ) ) ;
#9793 = CARTESIAN_POINT ( 'NONE',  ( 15.91767397667355155, 149.1530343478547422, 49.99999999999999289 ) ) ;
#9794 = DIRECTION ( 'NONE',  ( -0.000000000000000000, -0.000000000000000000, -1.000000000000000000 ) ) ;
#9795 = CIRCLE ( 'NONE', #962, 7.500000000000002665 ) ;
#9796 = CARTESIAN_POINT ( 'NONE',  ( -5.729042578294540888, -0.2993243175132380696, 293.5832628385307999 ) ) ;
#9797 = EDGE_CURVE ( 'NONE', #14568, #15800, #7822, .T. ) ;
#9798 = LINE ( 'NONE', #17985, #5798 ) ;
#9799 = PLANE ( 'NONE',  #3682 ) ;
#9800 = AXIS2_PLACEMENT_3D ( 'NONE', #3488, #1654, #19052 ) ;
#9801 = CARTESIAN_POINT ( 'NONE',  ( 91.69714670201405227, -118.7099181436120290, 47.50740515561367516 ) ) ;
#9802 = EDGE_LOOP ( 'NONE', ( #8917, #2045, #15625, #13819 ) ) ;
#9803 = CARTESIAN_POINT ( 'NONE',  ( 60.00000000000000711, 6.284666409917639535E-13, -100.0000000000000000 ) ) ;
#9804 = VERTEX_POINT ( 'NONE', #6307 ) ;
#9805 = ADVANCED_FACE ( 'NONE', ( #18575 ), #1285, .T. ) ;
#9806 = ORIENTED_EDGE ( 'NONE', *, *, #14317, .F. ) ;
#9807 = DIRECTION ( 'NONE',  ( 0.000000000000000000, 0.000000000000000000, 1.000000000000000000 ) ) ;
#9808 = VERTEX_POINT ( 'NONE', #10788 ) ;
#9809 = CIRCLE ( 'NONE', #13069, 7.500000000000007105 ) ;
#9810 = LINE ( 'NONE', #19233, #16982 ) ;
#9811 = LINE ( 'NONE', #11241, #7963 ) ;
#9812 = VERTEX_POINT ( 'NONE', #7920 ) ;
#9813 = FILL_AREA_STYLE ('',( #14325 ) ) ;
#9814 = DIRECTION ( 'NONE',  ( -6.982962677686266711E-15, 0.000000000000000000, -1.000000000000000000 ) ) ;
#9815 = LINE ( 'NONE', #2053, #12103 ) ;
#9816 = PRODUCT_DEFINITION_SHAPE ( 'NONE', 'NONE',  #19034 ) ;
#9817 = CARTESIAN_POINT ( 'NONE',  ( 102.6638558517306734, -126.6149147318370609, 1.229818221047174420 ) ) ;
#9818 = CARTESIAN_POINT ( 'NONE',  ( 159.9599531637113330, -36.50981547336952104, 49.99999999999999289 ) ) ;
#9819 = DIRECTION ( 'NONE',  ( 0.9271237148521548344, -0.3747554100459928317, 0.000000000000000000 ) ) ;
#9820 = CARTESIAN_POINT ( 'NONE',  ( 78.26059000578312919, -0.8220851292427129309, 112.7772637782949516 ) ) ;
#9821 = CARTESIAN_POINT ( 'NONE',  ( -56.84754764479025368, -154.7316448359455308, 39.99999999999999289 ) ) ;
#9822 = DIRECTION ( 'NONE',  ( 1.000000000000000000, 0.000000000000000000, 0.000000000000000000 ) ) ;
#9823 = AXIS2_PLACEMENT_3D ( 'NONE', #5718, #20105, #1598 ) ;
#9824 = CARTESIAN_POINT ( 'NONE',  ( 96.60517994339912207, -114.8199649187202880, 36.24366236571611921 ) ) ;
#9825 = ORIENTED_EDGE ( 'NONE', *, *, #19887, .T. ) ;
#9826 = CARTESIAN_POINT ( 'NONE',  ( 20.69304990905149211, 6.063840362151302621, 248.9926560891072143 ) ) ;
#9827 = CARTESIAN_POINT ( 'NONE',  ( -72.91900756452172061, 131.0832496385607158, -10.00000000000000178 ) ) ;
#9828 = ORIENTED_EDGE ( 'NONE', *, *, #16624, .F. ) ;
#9829 = ADVANCED_FACE ( 'NONE', ( #12524 ), #20099, .F. ) ;
#9830 = ORIENTED_EDGE ( 'NONE', *, *, #5175, .T. ) ;
#9831 = VERTEX_POINT ( 'NONE', #9155 ) ;
#9832 = EDGE_LOOP ( 'NONE', ( #18179, #4866, #9911 ) ) ;
#9833 = VECTOR ( 'NONE', #19507, 1000.000000000000114 ) ;
#9834 = DIRECTION ( 'NONE',  ( -0.3420201433256725987, 0.9396926207859068736, 0.000000000000000000 ) ) ;
#9835 = ORIENTED_EDGE ( 'NONE', *, *, #18888, .T. ) ;
#9836 = AXIS2_PLACEMENT_3D ( 'NONE', #18558, #10771, #19979 ) ;
#9837 =( NAMED_UNIT ( * ) PLANE_ANGLE_UNIT ( ) SI_UNIT ( $, .RADIAN. ) );
#9838 = CARTESIAN_POINT ( 'NONE',  ( 0.000000000000000000, 0.000000000000000000, 0.000000000000000000 ) ) ;
#9839 = CARTESIAN_POINT ( 'NONE',  ( -97.58443926496194365, -133.8443912861145009, 8.507479503170321422 ) ) ;
#9840 = ORIENTED_EDGE ( 'NONE', *, *, #1482, .F. ) ;
#9841 = EDGE_CURVE ( 'NONE', #3178, #15284, #8796, .T. ) ;
#9842 = DIRECTION ( 'NONE',  ( -0.7660444431189857850, -0.6427876096865300370, 5.348151281215662765E-15 ) ) ;
#9843 = AXIS2_PLACEMENT_3D ( 'NONE', #18871, #11285, #338 ) ;
#9844 = PLANE ( 'NONE',  #7580 ) ;
#9845 = CARTESIAN_POINT ( 'NONE',  ( 60.83768308848375739, -49.24833719034207036, 132.4711112102474146 ) ) ;
#9846 = DIRECTION ( 'NONE',  ( 1.000000000000000000, 0.000000000000000000, -0.000000000000000000 ) ) ;
#9847 = DIRECTION ( 'NONE',  ( 0.000000000000000000, 3.338476886082585705E-16, -1.000000000000000000 ) ) ;
#9848 = ORIENTED_EDGE ( 'NONE', *, *, #5556, .F. ) ;
#9849 = CARTESIAN_POINT ( 'NONE',  ( -136.2592242320518210, 27.06617804205124500, -18.18972273333671907 ) ) ;
#9850 = AXIS2_PLACEMENT_3D ( 'NONE', #4840, #1558, #3198 ) ;
#9851 = EDGE_CURVE ( 'NONE', #13843, #12327, #7516, .T. ) ;
#9852 = EDGE_CURVE ( 'NONE', #1374, #2759, #7175, .T. ) ;
#9853 = VERTEX_POINT ( 'NONE', #17247 ) ;
#9854 = APPLICATION_CONTEXT ( 'automotive_design' ) ;
#9855 = ORIENTED_EDGE ( 'NONE', *, *, #6042, .T. ) ;
#9856 = ORIENTED_EDGE ( 'NONE', *, *, #12411, .F. ) ;
#9857 = DIRECTION ( 'NONE',  ( -0.5060387318153625191, 0.000000000000000000, -0.8625107546591518348 ) ) ;
#9858 = CARTESIAN_POINT ( 'NONE',  ( 0.000000000000000000, 0.000000000000000000, 283.5832628385307999 ) ) ;
#9859 = ADVANCED_FACE ( 'NONE', ( #5998 ), #15504, .T. ) ;
#9860 = DIRECTION ( 'NONE',  ( -0.6427876096865430267, 0.7660444431189749048, 0.000000000000000000 ) ) ;
#9861 = EDGE_CURVE ( 'NONE', #5289, #3058, #6202, .T. ) ;
#9862 = CARTESIAN_POINT ( 'NONE',  ( 0.5612050131687996712, 4.355613924421553484, -9.000000000000001776 ) ) ;
#9863 = EDGE_CURVE ( 'NONE', #5705, #17978, #12217, .T. ) ;
#9864 = DIRECTION ( 'NONE',  ( 0.000000000000000000, 0.000000000000000000, -1.000000000000000000 ) ) ;
#9865 = FACE_OUTER_BOUND ( 'NONE', #2636, .T. ) ;
#9866 = FACE_BOUND ( 'NONE', #10441, .T. ) ;
#9867 = AXIS2_PLACEMENT_3D ( 'NONE', #12502, #3210, #12911 ) ;
#9868 = CARTESIAN_POINT ( 'NONE',  ( 0.000000000000000000, 0.000000000000000000, -115.0000000000000000 ) ) ;
#9869 = CARTESIAN_POINT ( 'NONE',  ( 100.5989061668482520, 55.02415981988612970, 14.88498244535475123 ) ) ;
#9870 = VERTEX_POINT ( 'NONE', #4874 ) ;
#9871 = PLANE ( 'NONE',  #8379 ) ;
#9872 = VERTEX_POINT ( 'NONE', #9261 ) ;
#9873 = EDGE_CURVE ( 'NONE', #16155, #15471, #15336, .T. ) ;
#9874 = ORIENTED_EDGE ( 'NONE', *, *, #17847, .F. ) ;
#9875 = EDGE_CURVE ( 'NONE', #4545, #5829, #4665, .T. ) ;
#9876 = ORIENTED_EDGE ( 'NONE', *, *, #15198, .F. ) ;
#9877 = VERTEX_POINT ( 'NONE', #9467 ) ;
#9878 = PLANE ( 'NONE',  #11213 ) ;
#9879 = AXIS2_PLACEMENT_3D ( 'NONE', #4861, #17344, #11772 ) ;
#9880 = CIRCLE ( 'NONE', #3683, 62.91752772691707207 ) ;
#9881 = ORIENTED_EDGE ( 'NONE', *, *, #17752, .T. ) ;
#9882 = CARTESIAN_POINT ( 'NONE',  ( -176.1792632384392050, -186.5724904703759535, 10.00000000000000178 ) ) ;
#9883 = CARTESIAN_POINT ( 'NONE',  ( -38.78191089773041256, 44.07268132743711675, 110.7293897666001214 ) ) ;
#9884 = DIRECTION ( 'NONE',  ( 0.000000000000000000, 1.000000000000000000, 0.000000000000000000 ) ) ;
#9885 = CARTESIAN_POINT ( 'NONE',  ( -1.396592535537253342E-14, 0.000000000000000000, 39.88498244535545467 ) ) ;
#9886 = VERTEX_POINT ( 'NONE', #9362 ) ;
#9887 = EDGE_CURVE ( 'NONE', #1021, #1356, #15710, .T. ) ;
#9888 = AXIS2_PLACEMENT_3D ( 'NONE', #8492, #10028, #19536 ) ;
#9889 = DIRECTION ( 'NONE',  ( -0.000000000000000000, -0.000000000000000000, -1.000000000000000000 ) ) ;
#9890 = DIRECTION ( 'NONE',  ( 1.000000000000000000, 0.000000000000000000, 0.000000000000000000 ) ) ;
#9891 = ADVANCED_FACE ( 'NONE', ( #4768 ), #13857, .T. ) ;
#9892 = EDGE_CURVE ( 'NONE', #5311, #15181, #12314, .T. ) ;
#9893 = ORIENTED_EDGE ( 'NONE', *, *, #4142, .F. ) ;
#9894 = EDGE_CURVE ( 'NONE', #10980, #2833, #17146, .T. ) ;
#9895 = CYLINDRICAL_SURFACE ( 'NONE', #13258, 7.500000000000007105 ) ;
#9896 = CARTESIAN_POINT ( 'NONE',  ( -15.91767397667354800, 149.1530343478547422, 39.99999999999999289 ) ) ;
#9897 = CARTESIAN_POINT ( 'NONE',  ( 0.000000000000000000, 0.000000000000000000, 132.4711112102474146 ) ) ;
#9898 = CARTESIAN_POINT ( 'NONE',  ( -134.5432410141372941, -66.31847138156592791, 36.21250959424132532 ) ) ;
#9899 = VECTOR ( 'NONE', #11260, 1000.000000000000000 ) ;
#9900 = VECTOR ( 'NONE', #4994, 1000.000000000000114 ) ;
#9901 = DIRECTION ( 'NONE',  ( 0.000000000000000000, 0.000000000000000000, 1.000000000000000000 ) ) ;
#9902 = CARTESIAN_POINT ( 'NONE',  ( 39.80940113486020948, -48.72193424476463974, 248.9926560891072143 ) ) ;
#9903 = CARTESIAN_POINT ( 'NONE',  ( -75.56543138647906233, 117.8553135366936147, -1.280227956710139781 ) ) ;
#9904 = ORIENTED_EDGE ( 'NONE', *, *, #4094, .F. ) ;
#9905 = EDGE_CURVE ( 'NONE', #3058, #2439, #9763, .T. ) ;
#9906 = CARTESIAN_POINT ( 'NONE',  ( -67.36461649554505016, 39.84224160888970800, 248.9926560891072143 ) ) ;
#9907 = ORIENTED_EDGE ( 'NONE', *, *, #2589, .T. ) ;
#9908 = VECTOR ( 'NONE', #19229, 1000.000000000000000 ) ;
#9909 = ORIENTED_EDGE ( 'NONE', *, *, #5050, .T. ) ;
#9910 = CARTESIAN_POINT ( 'NONE',  ( -110.0000000000000142, 275.0000000000000000, 5.000000000000000888 ) ) ;
#9911 = ORIENTED_EDGE ( 'NONE', *, *, #12889, .T. ) ;
#9912 = DIRECTION ( 'NONE',  ( 1.000000000000000000, 0.000000000000000000, -0.000000000000000000 ) ) ;
#9913 = DIRECTION ( 'NONE',  ( 0.000000000000000000, 0.000000000000000000, -1.000000000000000000 ) ) ;
#9914 = CIRCLE ( 'NONE', #17441, 62.91752772691707207 ) ;
#9915 = EDGE_CURVE ( 'NONE', #11866, #11373, #3021, .T. ) ;
#9916 = EDGE_CURVE ( 'NONE', #8891, #13644, #14688, .T. ) ;
#9917 = CARTESIAN_POINT ( 'NONE',  ( -52.50000000000000000, -2.094888803305880013E-13, -115.0000000000000000 ) ) ;
#9918 = DIRECTION ( 'NONE',  ( 0.7430374143461900838, -0.6692498792541753394, 0.000000000000000000 ) ) ;
#9919 = CYLINDRICAL_SURFACE ( 'NONE', #13597, 79.75827554147308263 ) ;
#9920 = DIRECTION ( 'NONE',  ( 1.000000000000000000, 0.000000000000000000, 0.000000000000000000 ) ) ;
#9921 = VECTOR ( 'NONE', #14490, 1000.000000000000000 ) ;
#9922 = EDGE_CURVE ( 'NONE', #12362, #4372, #14574, .T. ) ;
#9923 = DIRECTION ( 'NONE',  ( 6.982962677686266711E-15, -0.000000000000000000, 1.000000000000000000 ) ) ;
#9924 = FACE_OUTER_BOUND ( 'NONE', #20101, .T. ) ;
#9925 = PLANE ( 'NONE',  #11531 ) ;
#9926 = VECTOR ( 'NONE', #6455, 1000.000000000000114 ) ;
#9927 = CARTESIAN_POINT ( 'NONE',  ( 0.000000000000000000, 0.000000000000000000, 293.5832628385307999 ) ) ;
#9928 = LINE ( 'NONE', #14827, #3932 ) ;
#9929 = CARTESIAN_POINT ( 'NONE',  ( 103.5930306437996364, -125.1526588151300814, 39.21025145423357827 ) ) ;
#9930 = VERTEX_POINT ( 'NONE', #3429 ) ;
#9931 = DIRECTION ( 'NONE',  ( 0.9009688679024154823, 0.4338837391175657809, 0.000000000000000000 ) ) ;
#9932 = CARTESIAN_POINT ( 'NONE',  ( -63.98537287693041264, 94.20918150411493741, 14.88498244535589876 ) ) ;
#9933 = EDGE_LOOP ( 'NONE', ( #4158, #7307, #18644, #9166 ) ) ;
#9934 = ORIENTED_EDGE ( 'NONE', *, *, #8615, .T. ) ;
#9935 = ORIENTED_EDGE ( 'NONE', *, *, #480, .T. ) ;
#9936 = SHAPE_DEFINITION_REPRESENTATION ( #2155, #6269 ) ;
#9937 = AXIS2_PLACEMENT_3D ( 'NONE', #9443, #10761, #7690 ) ;
#9938 = ORIENTED_EDGE ( 'NONE', *, *, #8615, .F. ) ;
#9939 = ORIENTED_EDGE ( 'NONE', *, *, #18417, .T. ) ;
#9940 = CARTESIAN_POINT ( 'NONE',  ( -59.39925916207558743, -20.74471755083584057, 293.5832628385307999 ) ) ;
#9941 = VECTOR ( 'NONE', #3327, 1000.000000000000114 ) ;
#9942 = ORIENTED_EDGE ( 'NONE', *, *, #5050, .F. ) ;
#9943 = DIRECTION ( 'NONE',  ( 0.000000000000000000, 0.000000000000000000, -1.000000000000000000 ) ) ;
#9944 = CARTESIAN_POINT ( 'NONE',  ( -59.39925916207559453, -20.74471755083585478, 248.9926560891072143 ) ) ;
#9945 = CARTESIAN_POINT ( 'NONE',  ( -95.72167172977317762, -116.1306513017113957, 9.110179581664221260 ) ) ;
#9946 = VERTEX_POINT ( 'NONE', #254 ) ;
#9947 = CARTESIAN_POINT ( 'NONE',  ( -139.3985923533142284, -13.22154594654577231, 24.00007470227639317 ) ) ;
#9948 = FACE_OUTER_BOUND ( 'NONE', #2663, .T. ) ;
#9949 = CARTESIAN_POINT ( 'NONE',  ( 0.000000000000000000, 0.000000000000000000, 293.5832628385307999 ) ) ;
#9950 = CARTESIAN_POINT ( 'NONE',  ( -29.99999999999887379, 285.0000000000000568, 12.49999999999916511 ) ) ;
#9951 = AXIS2_PLACEMENT_3D ( 'NONE', #6155, #15559, #15452 ) ;
#9952 = CARTESIAN_POINT ( 'NONE',  ( -39.84224160888947353, -67.36461649554519227, 132.4711112102474146 ) ) ;
#9953 = DIRECTION ( 'NONE',  ( -0.000000000000000000, -1.000000000000000000, -0.000000000000000000 ) ) ;
#9954 = CARTESIAN_POINT ( 'NONE',  ( -54.89456854707564304, -30.74413178637171740, 248.9926560891072143 ) ) ;
#9955 = ORIENTED_EDGE ( 'NONE', *, *, #4320, .T. ) ;
#9956 = CARTESIAN_POINT ( 'NONE',  ( 56.84754764479241373, -154.7316448359447634, 49.99999999999999289 ) ) ;
#9957 = VECTOR ( 'NONE', #13829, 1000.000000000000000 ) ;
#9958 = VERTEX_POINT ( 'NONE', #4973 ) ;
#9959 = AXIS2_PLACEMENT_3D ( 'NONE', #4297, #19841, #18118 ) ;
#9960 = ORIENTED_EDGE ( 'NONE', *, *, #16466, .F. ) ;
#9961 = EDGE_LOOP ( 'NONE', ( #4781, #6200, #18126, #6619 ) ) ;
#9962 = AXIS2_PLACEMENT_3D ( 'NONE', #13633, #7106, #10562 ) ;
#9963 = CARTESIAN_POINT ( 'NONE',  ( -73.82206860051547892, -25.99419088092166774, 132.4711112102474146 ) ) ;
#9964 = DIRECTION ( 'NONE',  ( -0.7660444431189749048, -0.6427876096865430267, 0.000000000000000000 ) ) ;
#9965 = FACE_OUTER_BOUND ( 'NONE', #12256, .T. ) ;
#9966 = CARTESIAN_POINT ( 'NONE',  ( 6.352747104407250078E-17, 0.4400770685579608044, -9.000000000000000000 ) ) ;
#9967 = EDGE_CURVE ( 'NONE', #269, #13358, #5271, .T. ) ;
#9968 = CARTESIAN_POINT ( 'NONE',  ( -87.10655032386719654, -147.8252249328922687, 49.99999999999999289 ) ) ;
#9969 = CARTESIAN_POINT ( 'NONE',  ( -15.91767397667354800, 164.0736214083062805, 49.99999999999999289 ) ) ;
#9970 = LINE ( 'NONE', #5276, #394 ) ;
#9971 = DIRECTION ( 'NONE',  ( 0.000000000000000000, 0.000000000000000000, 1.000000000000000000 ) ) ;
#9972 = CARTESIAN_POINT ( 'NONE',  ( 104.1536737562094288, -124.2508859553631311, 39.42722059334807483 ) ) ;
#9973 = CIRCLE ( 'NONE', #1140, 7.500000000000007105 ) ;
#9974 = DIRECTION ( 'NONE',  ( -0.2080686897406911207, -0.9781142164131917394, 0.000000000000000000 ) ) ;
#9975 = EDGE_LOOP ( 'NONE', ( #15334, #16282, #8733, #6994 ) ) ;
#9976 = EDGE_LOOP ( 'NONE', ( #5088, #15101, #5265, #2633 ) ) ;
#9977 = ORIENTED_EDGE ( 'NONE', *, *, #7383, .F. ) ;
#9978 = EDGE_CURVE ( 'NONE', #16923, #2793, #8026, .T. ) ;
#9979 = ORIENTED_EDGE ( 'NONE', *, *, #11979, .F. ) ;
#9980 = EDGE_CURVE ( 'NONE', #3734, #16123, #16215, .T. ) ;
#9981 = AXIS2_PLACEMENT_3D ( 'NONE', #4432, #2905, #9133 ) ;
#9982 = VERTEX_POINT ( 'NONE', #14376 ) ;
#9983 = EDGE_CURVE ( 'NONE', #7218, #5595, #8431, .T. ) ;
#9984 = LINE ( 'NONE', #11318, #16781 ) ;
#9985 = VERTEX_POINT ( 'NONE', #461 ) ;
#9986 = LINE ( 'NONE', #3841, #2711 ) ;
#9987 = FACE_BOUND ( 'NONE', #14707, .T. ) ;
#9988 = CARTESIAN_POINT ( 'NONE',  ( 106.6880305650188063, 105.4403344747995845, 49.99999999999999289 ) ) ;
#9989 = ORIENTED_EDGE ( 'NONE', *, *, #11769, .T. ) ;
#9990 = CARTESIAN_POINT ( 'NONE',  ( 1.396592535537253342E-14, 0.000000000000000000, 43.88498244535545467 ) ) ;
#9991 = LINE ( 'NONE', #11524, #5211 ) ;
#9992 = ADVANCED_FACE ( 'NONE', ( #6904 ), #6807, .F. ) ;
#9993 = ORIENTED_EDGE ( 'NONE', *, *, #14981, .F. ) ;
#9994 = DIRECTION ( 'NONE',  ( -0.9271237148521536131, 0.3747554100459959958, 0.000000000000000000 ) ) ;
#9995 = DIRECTION ( 'NONE',  ( -1.000000000000000000, 0.000000000000000000, 6.976128451377903642E-15 ) ) ;
#9996 = FACE_OUTER_BOUND ( 'NONE', #5324, .T. ) ;
#9997 = VECTOR ( 'NONE', #4851, 1000.000000000000000 ) ;
#9998 = DIRECTION ( 'NONE',  ( 1.000000000000000000, 0.000000000000000000, 0.000000000000000000 ) ) ;
#9999 = DIRECTION ( 'NONE',  ( 0.3747554100459959958, 0.9271237148521535021, 0.000000000000000000 ) ) ;
#10000 = LINE ( 'NONE', #11915, #12284 ) ;
#10001 = ORIENTED_EDGE ( 'NONE', *, *, #7035, .F. ) ;
#10002 = VECTOR ( 'NONE', #5923, 1000.000000000000000 ) ;
#10003 = EDGE_CURVE ( 'NONE', #16270, #6781, #5369, .T. ) ;
#10004 = FACE_OUTER_BOUND ( 'NONE', #17864, .T. ) ;
#10005 = EDGE_LOOP ( 'NONE', ( #7833, #5266, #15276, #12876 ) ) ;
#10006 = EDGE_CURVE ( 'NONE', #9930, #5962, #10118, .T. ) ;
#10007 = ORIENTED_EDGE ( 'NONE', *, *, #19711, .T. ) ;
#10008 = EDGE_CURVE ( 'NONE', #13410, #15182, #9665, .T. ) ;
#10009 = CARTESIAN_POINT ( 'NONE',  ( -51.23821591265114961, -28.63313560863453944, 110.9660488491356887 ) ) ;
#10010 = VERTEX_POINT ( 'NONE', #15913 ) ;
#10011 = VECTOR ( 'NONE', #14993, 1000.000000000000000 ) ;
#10012 = DIRECTION ( 'NONE',  ( -0.7818314824680226982, -0.6234898018587423651, 0.000000000000000000 ) ) ;
#10013 = CLOSED_SHELL ( 'NONE', ( #4955, #4776, #19780, #12525, #7591, #6301, #12271, #18548, #15011, #16597, #11996, #847, #5479, #6369, #14614, #13087, #2015, #2874, #16021, #7671, #1782, #15932, #3243, #8502, #3229, #18775, #20053, #2769, #10896, #11731, #2302, #12765, #17270, #17920, #13220, #8510, #4749, #16146, #9223, #2177, #18251, #2172, #10965 ) ) ;
#10014 = LINE ( 'NONE', #13165, #3407 ) ;
#10015 = FACE_BOUND ( 'NONE', #9633, .T. ) ;
#10016 = CARTESIAN_POINT ( 'NONE',  ( -77.50000000000000000, 9.491012693391988181E-15, -105.0000000000000142 ) ) ;
#10017 = ORIENTED_EDGE ( 'NONE', *, *, #6606, .T. ) ;
#10018 = AXIS2_PLACEMENT_3D ( 'NONE', #13447, #693, #11811 ) ;
#10019 = EDGE_CURVE ( 'NONE', #9389, #2196, #11737, .T. ) ;
#10020 = CARTESIAN_POINT ( 'NONE',  ( 175.8776271403848739, -36.50981547336952104, 39.99999999999999289 ) ) ;
#10021 = CARTESIAN_POINT ( 'NONE',  ( -37.78198917157318704, 47.56244194535179304, 283.5832628385307999 ) ) ;
#10022 = CARTESIAN_POINT ( 'NONE',  ( 0.000000000000000000, 0.000000000000000000, 39.99999999999999289 ) ) ;
#10023 = CARTESIAN_POINT ( 'NONE',  ( 105.9946577255053626, 51.49356311920430329, 14.88498244535471215 ) ) ;
#10024 = VERTEX_POINT ( 'NONE', #1894 ) ;
#10025 = DIRECTION ( 'NONE',  ( 6.982962677686266711E-15, -0.000000000000000000, 1.000000000000000000 ) ) ;
#10026 = LINE ( 'NONE', #8684, #15248 ) ;
#10027 = CARTESIAN_POINT ( 'NONE',  ( 0.000000000000000000, 60.00000000000000000, -100.0000000000000000 ) ) ;
#10028 = DIRECTION ( 'NONE',  ( 0.000000000000000000, 0.000000000000000000, 1.000000000000000000 ) ) ;
#10029 = CIRCLE ( 'NONE', #9368, 7.500000000000001776 ) ;
#10030 = ORIENTED_EDGE ( 'NONE', *, *, #15787, .F. ) ;
#10031 = VECTOR ( 'NONE', #19264, 1000.000000000000227 ) ;
#10032 = DIRECTION ( 'NONE',  ( -0.000000000000000000, -0.000000000000000000, 1.000000000000000000 ) ) ;
#10033 = DIRECTION ( 'NONE',  ( 0.000000000000000000, 0.000000000000000000, 1.000000000000000000 ) ) ;
#10034 = EDGE_CURVE ( 'NONE', #13358, #5734, #3583, .T. ) ;
#10035 = VERTEX_POINT ( 'NONE', #8327 ) ;
#10036 = EDGE_CURVE ( 'NONE', #1970, #3220, #7494, .T. ) ;
#10037 = EDGE_CURVE ( 'NONE', #4265, #12970, #2694, .T. ) ;
#10038 = VERTEX_POINT ( 'NONE', #7391 ) ;
#10040 = ORIENTED_EDGE ( 'NONE', *, *, #3241, .T. ) ;
#10039 = AXIS2_PLACEMENT_3D ( 'NONE', #8187, #11152, #12580 ) ;
#10041 = APPLICATION_PROTOCOL_DEFINITION ( 'draft international standard', 'automotive_design', 1998, #2931 ) ;
#10042 = EDGE_CURVE ( 'NONE', #18312, #12789, #8533, .T. ) ;
#10043 = FACE_OUTER_BOUND ( 'NONE', #2763, .T. ) ;
#10044 = EDGE_LOOP ( 'NONE', ( #15687, #9460, #12967, #16777 ) ) ;
#10045 = DIRECTION ( 'NONE',  ( 0.7660444431189858960, -0.6427876096865300370, 0.000000000000000000 ) ) ;
#10046 = DIRECTION ( 'NONE',  ( 0.2080686897406943681, 0.9781142164131909622, 0.000000000000000000 ) ) ;
#10047 = CARTESIAN_POINT ( 'NONE',  ( -97.83472796452241482, -133.5146506974499232, 7.427686840538095581 ) ) ;
#10048 = ORIENTED_EDGE ( 'NONE', *, *, #9267, .F. ) ;
#10049 = B_SPLINE_CURVE_WITH_KNOTS ( 'NONE', 3,
 ( #3643, #9477, #12839, #19097, #266, #1700, #11311, #17259, #7931, #14183, #3238, #9675, #15823, #6716, #9577, #8139, #1805, #17568, #3441, #6520, #6316, #12742, #10999, #19001 ),
 .UNSPECIFIED., .F., .F.,
 ( 4, 2, 2, 2, 2, 2, 2, 2, 2, 2, 2, 4 ),
 ( 0.000000000000000000, 0.002919511036912160896, 0.005839022073824321792, 0.008758533110736483121, 0.01167804414764864358, 0.01313779966610474463, 0.01459755518456084568, 0.01751706622147301481, 0.01897682173992911239, 0.02043657725838521344, 0.02189633277684131102, 0.02335608829529741207 ),
 .UNSPECIFIED. ) ;
#10050 = CARTESIAN_POINT ( 'NONE',  ( -84.97262318625999455, -123.6115503146182277, -0.7768402190473889801 ) ) ;
#10051 = LINE ( 'NONE', #18217, #10257 ) ;
#10052 = AXIS2_PLACEMENT_3D ( 'NONE', #4281, #16762, #12249 ) ;
#10053 = DIRECTION ( 'NONE',  ( 0.000000000000000000, 1.000000000000000000, 0.000000000000000000 ) ) ;
#10054 = AXIS2_PLACEMENT_3D ( 'NONE', #17361, #6411, #18893 ) ;
#10055 = CARTESIAN_POINT ( 'NONE',  ( 53.87178215532755132, 28.06680738835045119, 283.5832628385307999 ) ) ;
#10056 = CARTESIAN_POINT ( 'NONE',  ( 48.17959877923549072, 36.99514631729036296, 293.5832628385307999 ) ) ;
#10057 = ORIENTED_EDGE ( 'NONE', *, *, #14050, .F. ) ;
#10058 = PLANE ( 'NONE',  #10063 ) ;
#10059 = LINE ( 'NONE', #13205, #11191 ) ;
#10060 = AXIS2_PLACEMENT_3D ( 'NONE', #15081, #13541, #1063 ) ;
#10061 = ORIENTED_EDGE ( 'NONE', *, *, #17555, .T. ) ;
#10062 = ADVANCED_FACE ( 'NONE', ( #5564 ), #11785, .T. ) ;
#10063 = AXIS2_PLACEMENT_3D ( 'NONE', #7280, #8811, #18127 ) ;
#10064 = EDGE_LOOP ( 'NONE', ( #19200, #6646, #500, #7933 ) ) ;
#10065 = LINE ( 'NONE', #9963, #2736 ) ;
#10066 = DIRECTION ( 'NONE',  ( 0.000000000000000000, 0.000000000000000000, 1.000000000000000000 ) ) ;
#10067 = LINE ( 'NONE', #19571, #15646 ) ;
#10068 = PLANE ( 'NONE',  #7819 ) ;
#10069 = FACE_OUTER_BOUND ( 'NONE', #12669, .T. ) ;
#10070 = DIRECTION ( 'NONE',  ( 1.000000000000000000, 0.000000000000000000, 0.000000000000000000 ) ) ;
#10071 = CARTESIAN_POINT ( 'NONE',  ( 133.1725405177770369, -69.15900471361744906, 7.877401435139040231 ) ) ;
#10072 = CIRCLE ( 'NONE', #8161, 112.8770930172170495 ) ;
#10073 = CYLINDRICAL_SURFACE ( 'NONE', #12109, 7.500000000000020428 ) ;
#10074 = CARTESIAN_POINT ( 'NONE',  ( 68.18670162478805707, 38.41834839689404646, 248.9926560891072143 ) ) ;
#10075 = AXIS2_PLACEMENT_3D ( 'NONE', #9305, #14319, #7966 ) ;
#10076 = PRODUCT_DEFINITION_CONTEXT ( 'detailed design', #6727, 'design' ) ;
#10077 = ORIENTED_EDGE ( 'NONE', *, *, #9922, .F. ) ;
#10078 = CIRCLE ( 'NONE', #1247, 15.91767397667354089 ) ;
#10079 = ORIENTED_EDGE ( 'NONE', *, *, #4117, .T. ) ;
#10080 = VERTEX_POINT ( 'NONE', #15167 ) ;
#10081 = EDGE_LOOP ( 'NONE', ( #14813, #15880, #8555, #16151 ) ) ;
#10082 = EDGE_CURVE ( 'NONE', #870, #12020, #8630, .T. ) ;
#10083 = VECTOR ( 'NONE', #16360, 1000.000000000000114 ) ;
#10084 = EDGE_LOOP ( 'NONE', ( #8384, #17130, #1491, #3443 ) ) ;
#10085 = CARTESIAN_POINT ( 'NONE',  ( 15.91767397667354800, 164.0736214083062805, 49.99999999999999289 ) ) ;
#10086 = CIRCLE ( 'NONE', #10719, 62.91752772691707207 ) ;
#10087 = CARTESIAN_POINT ( 'NONE',  ( 15.91767397667354089, 149.1530343478547422, 60.00000000000000000 ) ) ;
#10088 = AXIS2_PLACEMENT_3D ( 'NONE', #16639, #18269, #13441 ) ;
#10089 = DIRECTION ( 'NONE',  ( -0.5300553768524376430, -0.8479630283625698706, 0.000000000000000000 ) ) ;
#10090 = CARTESIAN_POINT ( 'NONE',  ( 0.000000000000000000, 0.000000000000000000, 293.5832628385307999 ) ) ;
#10091 = ORIENTED_EDGE ( 'NONE', *, *, #15498, .F. ) ;
#10092 = CARTESIAN_POINT ( 'NONE',  ( -18.77710619359115896, -55.62246070845775137, 132.4711112102474146 ) ) ;
#10093 = CARTESIAN_POINT ( 'NONE',  ( -26.42151830275515323, 4.658826548058537576, 14.88498244535563586 ) ) ;
#10094 = VERTEX_POINT ( 'NONE', #1149 ) ;
#10095 = DIRECTION ( 'NONE',  ( 0.6427876096865404731, -0.7660444431189771253, 0.000000000000000000 ) ) ;
#10096 = EDGE_CURVE ( 'NONE', #9086, #16353, #13369, .T. ) ;
#10097 = DIRECTION ( 'NONE',  ( -1.000000000000000000, 0.000000000000000000, 0.000000000000000000 ) ) ;
#10098 = DIRECTION ( 'NONE',  ( 1.000000000000000000, 0.000000000000000000, 0.000000000000000000 ) ) ;
#10099 = DIRECTION ( 'NONE',  ( 1.000000000000000000, 0.000000000000000000, 0.000000000000000000 ) ) ;
#10100 = VECTOR ( 'NONE', #17834, 1000.000000000000000 ) ;
#10101 = DIRECTION ( 'NONE',  ( -0.000000000000000000, -0.000000000000000000, -1.000000000000000000 ) ) ;
#10102 = CARTESIAN_POINT ( 'NONE',  ( -7.500000000000001776, 60.00000000000000000, -115.0000000000000000 ) ) ;
#10103 = DIRECTION ( 'NONE',  ( -0.9848077530122091305, 0.1736481776669241417, 0.000000000000000000 ) ) ;
#10104 = AXIS2_PLACEMENT_3D ( 'NONE', #12528, #8030, #17251 ) ;
#10105 = CIRCLE ( 'NONE', #14675, 7.500000000000003553 ) ;
#10106 = ORIENTED_EDGE ( 'NONE', *, *, #9145, .F. ) ;
#10107 = DIRECTION ( 'NONE',  ( 0.000000000000000000, 0.000000000000000000, -1.000000000000000000 ) ) ;
#10108 = ORIENTED_EDGE ( 'NONE', *, *, #3131, .F. ) ;
#10109 = ORIENTED_EDGE ( 'NONE', *, *, #9724, .F. ) ;
#10110 = ADVANCED_FACE ( 'NONE', ( #10258 ), #10068, .F. ) ;
#10111 = DIRECTION ( 'NONE',  ( 1.000000000000000000, 0.000000000000000000, 0.000000000000000000 ) ) ;
#10112 = ORIENTED_EDGE ( 'NONE', *, *, #8758, .F. ) ;
#10113 = DIRECTION ( 'NONE',  ( 0.6427876096865328126, 0.7660444431189835646, 0.000000000000000000 ) ) ;
#10114 = CARTESIAN_POINT ( 'NONE',  ( -82.17872144123516875, -125.4856950968008817, 32.52944088431316061 ) ) ;
#10115 = CYLINDRICAL_SURFACE ( 'NONE', #18484, 112.8770930172170210 ) ;
#10116 = DIRECTION ( 'NONE',  ( -0.7660444431189772363, 0.6427876096865402511, 4.304393070272779381E-15 ) ) ;
#10117 = VECTOR ( 'NONE', #14380, 1000.000000000000000 ) ;
#10118 = CIRCLE ( 'NONE', #5225, 60.74260934110282051 ) ;
#10119 = ORIENTED_EDGE ( 'NONE', *, *, #17449, .F. ) ;
#10120 = EDGE_CURVE ( 'NONE', #7092, #16671, #13522, .T. ) ;
#10121 = CARTESIAN_POINT ( 'NONE',  ( 0.000000000000000000, 0.000000000000000000, 0.000000000000000000 ) ) ;
#10122 = CARTESIAN_POINT ( 'NONE',  ( 97.49999999999997158, -133.9542832461880835, 9.515056863104252471 ) ) ;
#10123 = CARTESIAN_POINT ( 'NONE',  ( -3.123743752083691039, 4.811834253408552087, 283.5832628385307999 ) ) ;
#10124 = EDGE_CURVE ( 'NONE', #5311, #13590, #4554, .T. ) ;
#10125 = CARTESIAN_POINT ( 'NONE',  ( -25.47058595421602689, -74.01264520835145788, 132.4711112102474146 ) ) ;
#10126 = ORIENTED_EDGE ( 'NONE', *, *, #12501, .F. ) ;
#10127 = CYLINDRICAL_SURFACE ( 'NONE', #18730, 10.00000000000000888 ) ;
#10128 = CARTESIAN_POINT ( 'NONE',  ( 60.00000000000000711, 6.284666409917639535E-13, -105.0000000000000142 ) ) ;
#10129 = CARTESIAN_POINT ( 'NONE',  ( 99.70874217756774271, -112.0725815587889969, -9.999999999999996447 ) ) ;
#10130 = DIRECTION ( 'NONE',  ( -0.4999999999999979461, -0.8660254037844398178, 0.000000000000000000 ) ) ;
#10131 = ORIENTED_EDGE ( 'NONE', *, *, #8836, .F. ) ;
#10132 = PLANE ( 'NONE',  #10722 ) ;
#10133 = CYLINDRICAL_SURFACE ( 'NONE', #8581, 60.74260934110282051 ) ;
#10134 = ORIENTED_EDGE ( 'NONE', *, *, #4611, .T. ) ;
#10135 = ORIENTED_EDGE ( 'NONE', *, *, #8577, .F. ) ;
#10136 = EDGE_CURVE ( 'NONE', #5586, #5786, #10423, .T. ) ;
#10137 = CARTESIAN_POINT ( 'NONE',  ( -110.0000000000000142, 285.0000000000000568, -40.00000000000000711 ) ) ;
#10138 = VERTEX_POINT ( 'NONE', #5667 ) ;
#10139 = CARTESIAN_POINT ( 'NONE',  ( 107.5000000000000284, -118.5063289449133492, -3.469446951953614189E-15 ) ) ;
#10140 = CARTESIAN_POINT ( 'NONE',  ( -99.45845524092749201, -131.3126558323500319, 4.053310392242657656 ) ) ;
#10141 = VERTEX_POINT ( 'NONE', #16515 ) ;
#10142 = AXIS2_PLACEMENT_3D ( 'NONE', #1851, #12890, #19145 ) ;
#10143 = PRODUCT_DEFINITION_FORMATION_WITH_SPECIFIED_SOURCE ( 'ANY', '', #4, .NOT_KNOWN. ) ;
#10144 = EDGE_CURVE ( 'NONE', #17054, #9109, #6216, .T. ) ;
#10145 = VECTOR ( 'NONE', #3638, 1000.000000000000000 ) ;
#10146 = ADVANCED_FACE ( 'NONE', ( #17955 ), #2398, .F. ) ;
#10147 = PLANE ( 'NONE',  #3611 ) ;
#10148 = DIRECTION ( 'NONE',  ( -0.000000000000000000, -0.000000000000000000, 1.000000000000000000 ) ) ;
#10149 = CARTESIAN_POINT ( 'NONE',  ( 0.000000000000000000, 0.000000000000000000, 293.5832628385307999 ) ) ;
#10150 = DIRECTION ( 'NONE',  ( -1.000000000000000000, 0.000000000000000000, 6.977185866873309606E-15 ) ) ;
#10151 = LINE ( 'NONE', #16399, #5965 ) ;
#10152 = ORIENTED_EDGE ( 'NONE', *, *, #18096, .T. ) ;
#10153 = DIRECTION ( 'NONE',  ( 0.000000000000000000, 0.000000000000000000, -1.000000000000000000 ) ) ;
#10154 = CARTESIAN_POINT ( 'NONE',  ( 135.7779226595531270, 102.2982297021113141, 49.99999999999999289 ) ) ;
#10155 = VERTEX_POINT ( 'NONE', #16319 ) ;
#10156 = EDGE_CURVE ( 'NONE', #6223, #19500, #2493, .T. ) ;
#10157 = VECTOR ( 'NONE', #1367, 1000.000000000000000 ) ;
#10158 = VERTEX_POINT ( 'NONE', #18238 ) ;
#10159 = ORIENTED_EDGE ( 'NONE', *, *, #7505, .T. ) ;
#10160 = CARTESIAN_POINT ( 'NONE',  ( -12.23146955673647618, -77.31114765718488968, 112.0427633081292385 ) ) ;
#10161 = DIRECTION ( 'NONE',  ( 0.000000000000000000, 0.000000000000000000, 1.000000000000000000 ) ) ;
#10162 = DIRECTION ( 'NONE',  ( 0.3420201433256630508, 0.9396926207859104263, 0.000000000000000000 ) ) ;
#10163 = EDGE_CURVE ( 'NONE', #19981, #7250, #18625, .T. ) ;
#10164 = CARTESIAN_POINT ( 'NONE',  ( -73.25972925305610772, 27.53920554013711097, 132.4711112102474146 ) ) ;
#10165 = DIRECTION ( 'NONE',  ( 1.000000000000000000, 0.000000000000000000, 0.000000000000000000 ) ) ;
#10166 = CYLINDRICAL_SURFACE ( 'NONE', #17631, 77.50000000000000000 ) ;
#10167 = DIRECTION ( 'NONE',  ( 0.000000000000000000, 0.000000000000000000, 1.000000000000000000 ) ) ;
#10168 = VECTOR ( 'NONE', #407, 1000.000000000000227 ) ;
#10169 = CARTESIAN_POINT ( 'NONE',  ( 134.3401481871931651, -66.72943863802692022, 2.767325007884418930 ) ) ;
#10170 = LINE ( 'NONE', #5468, #18997 ) ;
#10171 = VECTOR ( 'NONE', #19273, 1000.000000000000000 ) ;
#10172 = CARTESIAN_POINT ( 'NONE',  ( 163.5019688434126977, -20.99123081650019884, 60.00000000000000000 ) ) ;
#10173 = ADVANCED_FACE ( 'NONE', ( #13315 ), #8725, .T. ) ;
#10174 = ORIENTED_EDGE ( 'NONE', *, *, #14282, .F. ) ;
#10175 = EDGE_LOOP ( 'NONE', ( #8140, #6113, #15851, #780 ) ) ;
#10176 = VERTEX_POINT ( 'NONE', #11883 ) ;
#10177 = ORIENTED_EDGE ( 'NONE', *, *, #20232, .F. ) ;
#10178 = DIRECTION ( 'NONE',  ( 0.000000000000000000, 0.000000000000000000, -1.000000000000000000 ) ) ;
#10179 = EDGE_LOOP ( 'NONE', ( #9542, #1239, #13570, #17214 ) ) ;
#10180 = CARTESIAN_POINT ( 'NONE',  ( 57.65577537092158877, -11.00103590902891249, 112.0427633081292385 ) ) ;
#10181 = CARTESIAN_POINT ( 'NONE',  ( 51.23821591265094355, 28.63313560863489471, 110.9660488491356887 ) ) ;
#10182 = CARTESIAN_POINT ( 'NONE',  ( -56.84754764479025368, -154.7316448359455308, 49.99999999999999289 ) ) ;
#10183 = ORIENTED_EDGE ( 'NONE', *, *, #3271, .F. ) ;
#10184 = AXIS2_PLACEMENT_3D ( 'NONE', #4959, #11074, #9744 ) ;
#10185 = LINE ( 'NONE', #14886, #15879 ) ;
#10186 = CARTESIAN_POINT ( 'NONE',  ( 59.42266395395792955, -50.93469132750283279, 110.7293897666001214 ) ) ;
#10187 = ORIENTED_EDGE ( 'NONE', *, *, #6982, .F. ) ;
#10188 = PLANE ( 'NONE',  #3571 ) ;
#10189 = DIRECTION ( 'NONE',  ( -0.000000000000000000, -0.000000000000000000, -1.000000000000000000 ) ) ;
#10190 = CARTESIAN_POINT ( 'NONE',  ( -134.3942145021295005, -75.36533733386917788, 5.353827179577918649 ) ) ;
#10191 = CARTESIAN_POINT ( 'NONE',  ( -110.0000000000000142, 285.0000000000000568, -75.00000000000000000 ) ) ;
#10192 = DIRECTION ( 'NONE',  ( -1.000000000000000000, 0.000000000000000000, 0.000000000000000000 ) ) ;
#10193 = PLANE ( 'NONE',  #10018 ) ;
#10194 = EDGE_LOOP ( 'NONE', ( #3779, #5355, #3094 ) ) ;
#10195 = DIRECTION ( 'NONE',  ( 0.000000000000000000, 1.000000000000000000, 0.000000000000000000 ) ) ;
#10196 = VECTOR ( 'NONE', #5209, 1000.000000000000000 ) ;
#10197 = VECTOR ( 'NONE', #2377, 1000.000000000000000 ) ;
#10198 = ORIENTED_EDGE ( 'NONE', *, *, #19474, .F. ) ;
#10199 = ORIENTED_EDGE ( 'NONE', *, *, #3016, .T. ) ;
#10200 = PLANE ( 'NONE',  #10543 ) ;
#10201 = ORIENTED_EDGE ( 'NONE', *, *, #5390, .F. ) ;
#10202 = VECTOR ( 'NONE', #1961, 1000.000000000000000 ) ;
#10203 = VECTOR ( 'NONE', #7780, 1000.000000000000000 ) ;
#10204 = CARTESIAN_POINT ( 'NONE',  ( 22.29928840491074382, 56.50138340076680521, 283.5832628385307999 ) ) ;
#10205 = CARTESIAN_POINT ( 'NONE',  ( 60.08127757648377099, 8.938941455415205795, 293.5832628385307999 ) ) ;
#10206 = CARTESIAN_POINT ( 'NONE',  ( 128.2779226595531270, 102.2982297021113141, 49.99999999999999289 ) ) ;
#10207 = DIRECTION ( 'NONE',  ( -0.000000000000000000, -0.000000000000000000, 1.000000000000000000 ) ) ;
#10208 = EDGE_LOOP ( 'NONE', ( #1607, #6718, #794, #15726 ) ) ;
#10209 = CYLINDRICAL_SURFACE ( 'NONE', #11956, 62.91752772691707207 ) ;
#10211 = CIRCLE ( 'NONE', #14468, 3.224098631618460331 ) ;
#10210 = LINE ( 'NONE', #8485, #5518 ) ;
#10212 = EDGE_CURVE ( 'NONE', #11724, #10980, #9795, .T. ) ;
#10213 = DIRECTION ( 'NONE',  ( -0.9993852124581887875, 0.03505990758545545621, 0.000000000000000000 ) ) ;
#10214 = LINE ( 'NONE', #16472, #5711 ) ;
#10215 = ORIENTED_EDGE ( 'NONE', *, *, #19993, .F. ) ;
#10216 = CARTESIAN_POINT ( 'NONE',  ( -28.63313560863435825, 51.23821591265124198, 248.9926560891072143 ) ) ;
#10217 = CARTESIAN_POINT ( 'NONE',  ( 98.63424005417277840, -113.0189783045208287, -9.902513086295204658 ) ) ;
#10218 = DIRECTION ( 'NONE',  ( -0.000000000000000000, -0.000000000000000000, -1.000000000000000000 ) ) ;
#10219 = ORIENTED_EDGE ( 'NONE', *, *, #3861, .F. ) ;
#10220 = LINE ( 'NONE', #19345, #3217 ) ;
#10221 = CARTESIAN_POINT ( 'NONE',  ( -34.51244174799990816, 110.9757759606085017, 14.88498244535569093 ) ) ;
#10222 = ORIENTED_EDGE ( 'NONE', *, *, #16363, .T. ) ;
#10223 = EDGE_CURVE ( 'NONE', #6348, #9156, #12297, .T. ) ;
#10224 = VERTEX_POINT ( 'NONE', #7693 ) ;
#10225 = EDGE_CURVE ( 'NONE', #14181, #1862, #3598, .T. ) ;
#10226 = AXIS2_PLACEMENT_3D ( 'NONE', #16454, #5597, #5214 ) ;
#10227 = MECHANICAL_DESIGN_GEOMETRIC_PRESENTATION_REPRESENTATION (  '', ( #11848 ), #6067 ) ;
#10228 = ADVANCED_FACE ( 'NONE', ( #1255 ), #18447, .T. ) ;
#10229 = EDGE_CURVE ( 'NONE', #16043, #7379, #10086, .T. ) ;
#10230 = DIRECTION ( 'NONE',  ( 0.3427509529624095941, 0.9394263059140722794, -0.000000000000000000 ) ) ;
#10231 = FACE_OUTER_BOUND ( 'NONE', #5165, .T. ) ;
#10232 = EDGE_LOOP ( 'NONE', ( #49, #8814, #15825, #17795 ) ) ;
#10233 = AXIS2_PLACEMENT_3D ( 'NONE', #17038, #5072, #456 ) ;
#10234 = CARTESIAN_POINT ( 'NONE',  ( -101.4383890160140425, -128.4709723833222768, 2.019278167221355780 ) ) ;
#10235 = APPLICATION_CONTEXT ( 'automotive_design' ) ;
#10236 = EDGE_CURVE ( 'NONE', #16933, #8290, #16810, .T. ) ;
#10237 = CARTESIAN_POINT ( 'NONE',  ( -138.8107028532319873, -18.39471665163164715, 24.88022817150739385 ) ) ;
#10238 = DIRECTION ( 'NONE',  ( -0.1736481776669404620, -0.9848077530122062440, 1.212578743696479242E-15 ) ) ;
#10239 = CYLINDRICAL_SURFACE ( 'NONE', #3362, 62.91752772691707207 ) ;
#10240 = CARTESIAN_POINT ( 'NONE',  ( -1.629865514042508456, -60.72073886220396588, 283.5832628385307999 ) ) ;
#10241 = CYLINDRICAL_SURFACE ( 'NONE', #9110, 7.500000000000000000 ) ;
#10242 = DIRECTION ( 'NONE',  ( 1.000000000000000000, 0.000000000000000000, 0.000000000000000000 ) ) ;
#10243 = VERTEX_POINT ( 'NONE', #10765 ) ;
#10244 = CARTESIAN_POINT ( 'NONE',  ( 2.605298826210336927, 5.111158570922247790, 283.5832628385307999 ) ) ;
#10245 = LINE ( 'NONE', #16503, #12503 ) ;
#10246 = VECTOR ( 'NONE', #6482, 1000.000000000000341 ) ;
#10247 = EDGE_LOOP ( 'NONE', ( #2357, #9496, #3250, #13021 ) ) ;
#10248 = VECTOR ( 'NONE', #11323, 1000.000000000000000 ) ;
#10249 = ADVANCED_FACE ( 'NONE', ( #5869 ), #13729, .T. ) ;
#10250 = ORIENTED_EDGE ( 'NONE', *, *, #3523, .F. ) ;
#10251 = EDGE_CURVE ( 'NONE', #11005, #11485, #4640, .T. ) ;
#10252 = DIRECTION ( 'NONE',  ( 0.000000000000000000, 0.000000000000000000, 1.000000000000000000 ) ) ;
#10253 = VERTEX_POINT ( 'NONE', #3006 ) ;
#10254 = DIRECTION ( 'NONE',  ( 1.000000000000000000, 0.000000000000000000, 0.000000000000000000 ) ) ;
#10255 = CARTESIAN_POINT ( 'NONE',  ( 25.47058595421554372, 74.01264520835162841, 111.4180192758974499 ) ) ;
#10256 = DIRECTION ( 'NONE',  ( -1.000000000000000000, -1.613511099790691498E-16, 0.000000000000000000 ) ) ;
#10257 = VECTOR ( 'NONE', #3805, 1000.000000000000000 ) ;
#10258 = FACE_OUTER_BOUND ( 'NONE', #19368, .T. ) ;
#10259 = VERTEX_POINT ( 'NONE', #9025 ) ;
#10260 = FACE_OUTER_BOUND ( 'NONE', #5813, .T. ) ;
#10261 = DIRECTION ( 'NONE',  ( -6.982962677686266711E-15, 0.000000000000000000, -1.000000000000000000 ) ) ;
#10262 = ADVANCED_FACE ( 'NONE', ( #6076, #12786 ), #15584, .T. ) ;
#10263 = DIRECTION ( 'NONE',  ( 1.000000000000000000, -0.000000000000000000, 0.000000000000000000 ) ) ;
#10264 = VECTOR ( 'NONE', #1485, 999.9999999999998863 ) ;
#10265 = CYLINDRICAL_SURFACE ( 'NONE', #8846, 62.91752772691707207 ) ;
#10266 = DIRECTION ( 'NONE',  ( -0.000000000000000000, -0.000000000000000000, 1.000000000000000000 ) ) ;
#10267 = DIRECTION ( 'NONE',  ( -0.000000000000000000, -0.000000000000000000, 1.000000000000000000 ) ) ;
#10268 = ORIENTED_EDGE ( 'NONE', *, *, #14683, .F. ) ;
#10269 = ORIENTED_EDGE ( 'NONE', *, *, #2128, .T. ) ;
#10270 = ORIENTED_EDGE ( 'NONE', *, *, #8404, .F. ) ;
#10271 = ADVANCED_FACE ( 'NONE', ( #14046 ), #19973, .T. ) ;
#10272 = AXIS2_PLACEMENT_3D ( 'NONE', #85, #491, #6737 ) ;
#10273 = ADVANCED_FACE ( 'NONE', ( #15372 ), #1361, .T. ) ;
#10274 = ORIENTED_EDGE ( 'NONE', *, *, #8214, .F. ) ;
#10275 = ORIENTED_EDGE ( 'NONE', *, *, #7033, .T. ) ;
#10276 = CARTESIAN_POINT ( 'NONE',  ( 70.38703763562291726, -92.47916748300480094, 39.88498244535495729 ) ) ;
#10277 = ADVANCED_FACE ( 'NONE', ( #5971 ), #17509, .T. ) ;
#10278 = CARTESIAN_POINT ( 'NONE',  ( -127.4413876050234933, 1.560706874093891490E-14, 39.88498244535634285 ) ) ;
#10279 = CYLINDRICAL_SURFACE ( 'NONE', #2553, 7.500000000000020428 ) ;
#10280 = ORIENTED_EDGE ( 'NONE', *, *, #14317, .T. ) ;
#10282 = CYLINDRICAL_SURFACE ( 'NONE', #6735, 140.0000000000000284 ) ;
#10281 = AXIS2_PLACEMENT_3D ( 'NONE', #9075, #2445, #11735 ) ;
#10283 = LINE ( 'NONE', #10186, #16320 ) ;
#10284 = ORIENTED_EDGE ( 'NONE', *, *, #18529, .F. ) ;
#10285 = CYLINDRICAL_SURFACE ( 'NONE', #10088, 15.91767397667354089 ) ;
#10286 = PLANE ( 'NONE',  #5138 ) ;
#10287 = DIRECTION ( 'NONE',  ( -0.000000000000000000, -0.000000000000000000, -1.000000000000000000 ) ) ;
#10288 = VECTOR ( 'NONE', #8833, 1000.000000000000114 ) ;
#10289 = DIRECTION ( 'NONE',  ( -0.7406645559057076778, -0.6718750000000006661, -0.000000000000000000 ) ) ;
#10290 = DIRECTION ( 'NONE',  ( -0.000000000000000000, -0.000000000000000000, 1.000000000000000000 ) ) ;
#10291 = CYLINDRICAL_SURFACE ( 'NONE', #10985, 3.224098631618460331 ) ;
#10292 = ORIENTED_EDGE ( 'NONE', *, *, #7366, .F. ) ;
#10293 = LINE ( 'NONE', #16351, #16776 ) ;
#10294 = ORIENTED_EDGE ( 'NONE', *, *, #17507, .T. ) ;
#10295 = ORIENTED_EDGE ( 'NONE', *, *, #4258, .T. ) ;
#10296 = DIRECTION ( 'NONE',  ( -0.4693298356057531429, 0.8830229359480288309, 0.000000000000000000 ) ) ;
#10297 = ORIENTED_EDGE ( 'NONE', *, *, #8528, .T. ) ;
#10298 = VERTEX_POINT ( 'NONE', #15268 ) ;
#10299 = DIRECTION ( 'NONE',  ( 0.000000000000000000, 0.000000000000000000, 1.000000000000000000 ) ) ;
#10300 = CARTESIAN_POINT ( 'NONE',  ( -21.73104181959847025, -16.26654594725001957, 14.88498244535560389 ) ) ;
#10301 = LINE ( 'NONE', #2248, #11612 ) ;
#10302 = DIRECTION ( 'NONE',  ( 0.000000000000000000, 0.000000000000000000, 1.000000000000000000 ) ) ;
#10303 = CIRCLE ( 'NONE', #4429, 112.8770930172170495 ) ;
#10304 = EDGE_LOOP ( 'NONE', ( #13512, #1879, #13546, #8473 ) ) ;
#10305 = DIRECTION ( 'NONE',  ( -0.000000000000000000, -0.000000000000000000, 1.000000000000000000 ) ) ;
#10306 = CARTESIAN_POINT ( 'NONE',  ( 32.50000000000000000, 0.000000000000000000, -110.0000000000000000 ) ) ;
#10307 = DIRECTION ( 'NONE',  ( 0.000000000000000000, 0.000000000000000000, 1.000000000000000000 ) ) ;
#10308 = LINE ( 'NONE', #19722, #14522 ) ;
#10309 = EDGE_LOOP ( 'NONE', ( #11805, #12954, #5189 ) ) ;
#10310 = DIRECTION ( 'NONE',  ( -0.3420201433256726542, 0.9396926207859068736, 0.000000000000000000 ) ) ;
#10311 = CARTESIAN_POINT ( 'NONE',  ( 84.32000978867640129, -124.0571233621914899, 0.4179024135772307358 ) ) ;
#10312 = DIRECTION ( 'NONE',  ( 1.047444401652940164E-14, -1.000000000000000000, 0.000000000000000000 ) ) ;
#10313 = VERTEX_POINT ( 'NONE', #12402 ) ;
#10314 = CARTESIAN_POINT ( 'NONE',  ( 60.22232964560483737, 7.948937137877944537, 293.5832628385307999 ) ) ;
#10315 = LINE ( 'NONE', #17916, #18383 ) ;
#10316 = VERTEX_POINT ( 'NONE', #1954 ) ;
#10317 = VECTOR ( 'NONE', #3774, 1000.000000000000227 ) ;
#10318 = ORIENTED_EDGE ( 'NONE', *, *, #37, .F. ) ;
#10319 = AXIS2_PLACEMENT_3D ( 'NONE', #10700, #13671, #19915 ) ;
#10320 = EDGE_LOOP ( 'NONE', ( #17532, #6420, #11775, #12493 ) ) ;
#10321 = EDGE_CURVE ( 'NONE', #7913, #1356, #926, .T. ) ;
#10322 = LINE ( 'NONE', #15039, #18573 ) ;
#10323 = AXIS2_PLACEMENT_3D ( 'NONE', #1829, #8061, #14312 ) ;
#10324 = DIRECTION ( 'NONE',  ( 0.000000000000000000, 0.000000000000000000, -1.000000000000000000 ) ) ;
#10325 = ORIENTED_EDGE ( 'NONE', *, *, #20142, .F. ) ;
#10326 = DIRECTION ( 'NONE',  ( -0.000000000000000000, -0.000000000000000000, 1.000000000000000000 ) ) ;
#10327 = CARTESIAN_POINT ( 'NONE',  ( -106.3852469178145412, -120.5001569748711461, 0.04619868349364349841 ) ) ;
#10328 = CARTESIAN_POINT ( 'NONE',  ( -136.4994460260996902, -31.11111111111111427, 27.86436879316430648 ) ) ;
#10329 = PLANE ( 'NONE',  #10569 ) ;
#10330 = CIRCLE ( 'NONE', #559, 60.74260934110282051 ) ;
#10331 = EDGE_CURVE ( 'NONE', #1274, #15008, #4428, .T. ) ;
#10332 = DIRECTION ( 'NONE',  ( -0.000000000000000000, -0.000000000000000000, 1.000000000000000000 ) ) ;
#10333 = DIRECTION ( 'NONE',  ( -0.000000000000000000, -0.000000000000000000, -1.000000000000000000 ) ) ;
#10334 = LINE ( 'NONE', #18033, #6957 ) ;
#10335 = ORIENTED_EDGE ( 'NONE', *, *, #2197, .F. ) ;
#10336 = ADVANCED_FACE ( 'NONE', ( #16913 ), #4876, .T. ) ;
#10337 = AXIS2_PLACEMENT_3D ( 'NONE', #4075, #5523, #16175 ) ;
#10338 = DIRECTION ( 'NONE',  ( 1.000000000000000000, 0.000000000000000000, 0.000000000000000000 ) ) ;
#10339 = CARTESIAN_POINT ( 'NONE',  ( 0.000000000000000000, 0.000000000000000000, 283.5832628385307999 ) ) ;
#10340 = ORIENTED_EDGE ( 'NONE', *, *, #4155, .F. ) ;
#10341 = ORIENTED_EDGE ( 'NONE', *, *, #11853, .T. ) ;
#10342 =( LENGTH_UNIT ( ) NAMED_UNIT ( * ) SI_UNIT ( .MILLI., .METRE. ) );
#10343 = ORIENTED_EDGE ( 'NONE', *, *, #15676, .T. ) ;
#10344 = ADVANCED_FACE ( 'NONE', ( #3108 ), #19238, .F. ) ;
#10345 = LINE ( 'NONE', #16601, #9020 ) ;
#10346 = EDGE_LOOP ( 'NONE', ( #10106, #7527, #8401, #4187 ) ) ;
#10347 = DIRECTION ( 'NONE',  ( -0.000000000000000000, -0.000000000000000000, -1.000000000000000000 ) ) ;
#10348 = VECTOR ( 'NONE', #18716, 1000.000000000000000 ) ;
#10349 = CARTESIAN_POINT ( 'NONE',  ( 107.5000000000000284, -199.9999999999999716, 0.000000000000000000 ) ) ;
#10350 = CARTESIAN_POINT ( 'NONE',  ( -99.33980890132491481, -112.3956798702028692, 39.16385526563716724 ) ) ;
#10351 = CARTESIAN_POINT ( 'NONE',  ( 113.5802308907675666, 8.308367629983374414, 14.88498244535465709 ) ) ;
#10352 = DIRECTION ( 'NONE',  ( -1.000000000000000000, 0.000000000000000000, 0.000000000000000000 ) ) ;
#10353 = FACE_OUTER_BOUND ( 'NONE', #2505, .T. ) ;
#10354 = CARTESIAN_POINT ( 'NONE',  ( -126.4587173007283809, -80.71184697946637243, -1.017284155395590250 ) ) ;
#10355 = EDGE_CURVE ( 'NONE', #11184, #16332, #4523, .T. ) ;
#10356 = LINE ( 'NONE', #2207, #18039 ) ;
#10357 = EDGE_CURVE ( 'NONE', #3818, #7363, #3971, .T. ) ;
#10358 = DIRECTION ( 'NONE',  ( 1.000000000000000000, 0.000000000000000000, 0.000000000000000000 ) ) ;
#10359 = CARTESIAN_POINT ( 'NONE',  ( 19.23677882349201695, -57.61823435390814296, 293.5832628385307999 ) ) ;
#10360 = CARTESIAN_POINT ( 'NONE',  ( -135.1060089016710037, -65.16414933582423430, 31.52442972994579051 ) ) ;
#10361 = EDGE_CURVE ( 'NONE', #9422, #8266, #5130, .T. ) ;
#10362 = AXIS2_PLACEMENT_3D ( 'NONE', #14396, #15935, #19109 ) ;
#10364 = ORIENTED_EDGE ( 'NONE', *, *, #17750, .T. ) ;
#10363 = AXIS2_PLACEMENT_3D ( 'NONE', #8712, #6615, #10338 ) ;
#10365 = ORIENTED_EDGE ( 'NONE', *, *, #1765, .T. ) ;
#10366 = ORIENTED_EDGE ( 'NONE', *, *, #14168, .F. ) ;
#10367 = EDGE_CURVE ( 'NONE', #6205, #1414, #15966, .T. ) ;
#10368 = VERTEX_POINT ( 'NONE', #10021 ) ;
#10369 = DIRECTION ( 'NONE',  ( 0.000000000000000000, 0.000000000000000000, -1.000000000000000000 ) ) ;
#10370 = DIRECTION ( 'NONE',  ( 1.000000000000000000, 0.000000000000000000, 0.000000000000000000 ) ) ;
#10371 = EDGE_LOOP ( 'NONE', ( #4991, #12289 ) ) ;
#10372 = DIRECTION ( 'NONE',  ( 0.4338837391175525693, 0.9009688679024216995, 0.000000000000000000 ) ) ;
#10373 = FACE_OUTER_BOUND ( 'NONE', #4572, .T. ) ;
#10374 = CIRCLE ( 'NONE', #261, 60.74260934110282051 ) ;
#10375 = ORIENTED_EDGE ( 'NONE', *, *, #15664, .T. ) ;
#10376 = FACE_OUTER_BOUND ( 'NONE', #15677, .T. ) ;
#10377 = FACE_OUTER_BOUND ( 'NONE', #5333, .T. ) ;
#10378 = CARTESIAN_POINT ( 'NONE',  ( -133.6841479863219604, -79.85751371701380208, 2.530482114511096281 ) ) ;
#10379 = EDGE_CURVE ( 'NONE', #4335, #9958, #10210, .T. ) ;
#10380 = LINE ( 'NONE', #16642, #9833 ) ;
#10381 = ADVANCED_FACE ( 'NONE', ( #2054 ), #11353, .T. ) ;
#10382 = EDGE_CURVE ( 'NONE', #17163, #14304, #19528, .T. ) ;
#10383 = EDGE_CURVE ( 'NONE', #10900, #14067, #14820, .T. ) ;
#10384 = LINE ( 'NONE', #4255, #7128 ) ;
#10385 = EDGE_LOOP ( 'NONE', ( #20143, #19083, #15925, #9756 ) ) ;
#10386 = DIRECTION ( 'NONE',  ( 1.000000000000000000, 0.000000000000000000, -0.000000000000000000 ) ) ;
#10387 = AXIS2_PLACEMENT_3D ( 'NONE', #8867, #12130, #15107 ) ;
#10388 = VERTEX_POINT ( 'NONE', #5517 ) ;
#10389 = AXIS2_PLACEMENT_3D ( 'NONE', #18445, #15165, #18344 ) ;
#10390 = VECTOR ( 'NONE', #4319, 999.9999999999998863 ) ;
#10391 = VERTEX_POINT ( 'NONE', #6757 ) ;
#10392 = LINE ( 'NONE', #11919, #4011 ) ;
#10393 = VECTOR ( 'NONE', #6512, 1000.000000000000000 ) ;
#10394 = ORIENTED_EDGE ( 'NONE', *, *, #17917, .F. ) ;
#10395 = VERTEX_POINT ( 'NONE', #17709 ) ;
#10396 = B_SPLINE_CURVE_WITH_KNOTS ( 'NONE', 3,
 ( #12675, #7767, #20047, #4604, #14109, #15658, #3176, #1536, #7868, #4498, #7969, #10827, #6349, #18833, #11037, #4925, #20149, #14007, #11140, #9308, #9609, #15858, #7561, #1651, #10729, #15550 ),
 .UNSPECIFIED., .F., .F.,
 ( 4, 2, 2, 2, 2, 2, 2, 2, 2, 2, 2, 2, 4 ),
 ( 0.06489813153835151394, 0.07443177014004152825, 0.07681517979046398326, 0.07919858944088645214, 0.08396540874173136215, 0.09349904734342115442, 0.1030326859451109606, 0.1077995052459558289, 0.1101829148963782701, 0.1125663245468007251, 0.1220999631484905035, 0.1316336017501802680, 0.1411672403518700325 ),
 .UNSPECIFIED. ) ;
#10397 = DIRECTION ( 'NONE',  ( -0.7071067811865472397, 8.659560562354930393E-17, 0.7071067811865479058 ) ) ;
#10398 = DIRECTION ( 'NONE',  ( -0.000000000000000000, -0.000000000000000000, 1.000000000000000000 ) ) ;
#10399 = LINE ( 'NONE', #12239, #4492 ) ;
#10400 = DIRECTION ( 'NONE',  ( 0.000000000000000000, 0.000000000000000000, 1.000000000000000000 ) ) ;
#10401 = CARTESIAN_POINT ( 'NONE',  ( -60.08127757648377099, -8.938941455415186255, 283.5832628385307999 ) ) ;
#10402 = VERTEX_POINT ( 'NONE', #3681 ) ;
#10403 = DIRECTION ( 'NONE',  ( -0.000000000000000000, -0.000000000000000000, -1.000000000000000000 ) ) ;
#10404 = DIRECTION ( 'NONE',  ( 0.000000000000000000, 0.000000000000000000, 1.000000000000000000 ) ) ;
#10405 = EDGE_CURVE ( 'NONE', #5526, #4062, #2270, .T. ) ;
#10406 = CIRCLE ( 'NONE', #12697, 34.99999999999997868 ) ;
#10407 = AXIS2_PLACEMENT_3D ( 'NONE', #1067, #16636, #1170 ) ;
#10408 = PLANE ( 'NONE',  #20075 ) ;
#10409 = VECTOR ( 'NONE', #8727, 1000.000000000000000 ) ;
#10410 = ORIENTED_EDGE ( 'NONE', *, *, #17035, .T. ) ;
#10411 = CARTESIAN_POINT ( 'NONE',  ( 38.41834839689379777, -68.18670162478818497, 248.9926560891072143 ) ) ;
#10412 = CARTESIAN_POINT ( 'NONE',  ( -134.1070788506806082, -77.29467090009929109, 36.09959090400466408 ) ) ;
#10413 = CYLINDRICAL_SURFACE ( 'NONE', #1727, 106.4288957539801004 ) ;
#10414 = EDGE_CURVE ( 'NONE', #7514, #18061, #8580, .T. ) ;
#10415 = ORIENTED_EDGE ( 'NONE', *, *, #2615, .T. ) ;
#10416 = FACE_BOUND ( 'NONE', #13242, .T. ) ;
#10417 = CARTESIAN_POINT ( 'NONE',  ( -110.0000000000000142, 165.0000000000000000, 5.000000000000000888 ) ) ;
#10418 = ORIENTED_EDGE ( 'NONE', *, *, #11538, .F. ) ;
#10419 = ORIENTED_EDGE ( 'NONE', *, *, #5112, .T. ) ;
#10420 = DIRECTION ( 'NONE',  ( -0.000000000000000000, -0.000000000000000000, 1.000000000000000000 ) ) ;
#10421 = ORIENTED_EDGE ( 'NONE', *, *, #18154, .T. ) ;
#10422 = VECTOR ( 'NONE', #11269, 1000.000000000000114 ) ;
#10423 = CIRCLE ( 'NONE', #15017, 7.500000000000007105 ) ;
#10424 = DIRECTION ( 'NONE',  ( 6.982962677686266711E-15, -0.000000000000000000, 1.000000000000000000 ) ) ;
#10425 = LINE ( 'NONE', #16682, #15581 ) ;
#10426 = ORIENTED_EDGE ( 'NONE', *, *, #19634, .F. ) ;
#10427 = DIRECTION ( 'NONE',  ( -0.3420201433256568335, -0.9396926207859126468, 0.000000000000000000 ) ) ;
#10428 = CARTESIAN_POINT ( 'NONE',  ( 56.84754764479240663, -154.7316448359447634, 39.99999999999999289 ) ) ;
#10429 = CARTESIAN_POINT ( 'NONE',  ( -137.8187983416405018, -24.47065216059271719, -13.51171419847062793 ) ) ;
#10430 = CARTESIAN_POINT ( 'NONE',  ( 0.000000000000000000, 0.000000000000000000, 283.5832628385307999 ) ) ;
#10431 = CARTESIAN_POINT ( 'NONE',  ( 103.2967819461768073, 53.25886146954521649, 14.88498244535472992 ) ) ;
#10432 = PLANE ( 'NONE',  #4663 ) ;
#10433 = DIRECTION ( 'NONE',  ( 1.000000000000000000, 0.000000000000000000, 0.000000000000000000 ) ) ;
#10434 = CARTESIAN_POINT ( 'NONE',  ( -67.50000000000000000, -2.085703952312275003E-13, -105.0000000000000142 ) ) ;
#10435 = DIRECTION ( 'NONE',  ( 0.000000000000000000, 0.000000000000000000, -1.000000000000000000 ) ) ;
#10436 = EDGE_LOOP ( 'NONE', ( #16406, #15620, #2537, #16625 ) ) ;
#10437 = DIRECTION ( 'NONE',  ( 0.000000000000000000, 1.000000000000000000, 0.000000000000000000 ) ) ;
#10438 = DIRECTION ( 'NONE',  ( 0.9848077530122097967, -0.1736481776669206722, 0.000000000000000000 ) ) ;
#10439 = ORIENTED_EDGE ( 'NONE', *, *, #10136, .T. ) ;
#10440 = ORIENTED_EDGE ( 'NONE', *, *, #20008, .F. ) ;
#10441 = EDGE_LOOP ( 'NONE', ( #6682, #12412 ) ) ;
#10442 = VECTOR ( 'NONE', #3266, 1000.000000000000000 ) ;
#10443 = CARTESIAN_POINT ( 'NONE',  ( -7.500000000000001776, 60.00000000000000000, -115.0000000000000000 ) ) ;
#10444 = VERTEX_POINT ( 'NONE', #408 ) ;
#10445 = CIRCLE ( 'NONE', #12741, 62.91752772691707207 ) ;
#10446 = CARTESIAN_POINT ( 'NONE',  ( 133.3655458879726723, -81.62736142943096240, 1.797406865988563807 ) ) ;
#10447 = CARTESIAN_POINT ( 'NONE',  ( -15.91767397667354800, 149.1530343478547138, 49.99999999999999289 ) ) ;
#10448 = DIRECTION ( 'NONE',  ( 0.000000000000000000, 1.000000000000000000, 0.000000000000000000 ) ) ;
#10449 = DIRECTION ( 'NONE',  ( -0.000000000000000000, -0.000000000000000000, 1.000000000000000000 ) ) ;
#10450 = VERTEX_POINT ( 'NONE', #11831 ) ;
#10451 = DIRECTION ( 'NONE',  ( -6.982962677686266711E-15, 0.000000000000000000, -1.000000000000000000 ) ) ;
#10452 = CARTESIAN_POINT ( 'NONE',  ( -134.3599121685007276, -75.61163470460564895, 5.100086963784538518 ) ) ;
#10453 = CARTESIAN_POINT ( 'NONE',  ( 69.11703934647968595, -95.44259730872654757, 39.88498244535497150 ) ) ;
#10454 = CARTESIAN_POINT ( 'NONE',  ( 7.500000000000420997, -60.00000000000000000, -100.0000000000000000 ) ) ;
#10455 = DIRECTION ( 'NONE',  ( -0.7881095627315619634, -0.6155349844899687950, 0.000000000000000000 ) ) ;
#10456 = CARTESIAN_POINT ( 'NONE',  ( 44.79940644582654841, -41.02350267428983699, 293.5832628385307999 ) ) ;
#10457 = ADVANCED_FACE ( 'NONE', ( #1001 ), #19925, .T. ) ;
#10458 = EDGE_LOOP ( 'NONE', ( #17766, #16693 ) ) ;
#10459 = ADVANCED_FACE ( 'NONE', ( #1314 ), #19822, .T. ) ;
#10460 = LINE ( 'NONE', #3757, #4660 ) ;
#10461 = VECTOR ( 'NONE', #19721, 1000.000000000000000 ) ;
#10462 = ORIENTED_EDGE ( 'NONE', *, *, #18275, .F. ) ;
#10463 = EDGE_LOOP ( 'NONE', ( #16404, #13688, #8172, #5246 ) ) ;
#10464 = ORIENTED_EDGE ( 'NONE', *, *, #4080, .T. ) ;
#10465 = EDGE_CURVE ( 'NONE', #17524, #3620, #13998, .T. ) ;
#10466 = VERTEX_POINT ( 'NONE', #16861 ) ;
#10467 = EDGE_CURVE ( 'NONE', #16270, #5054, #6823, .T. ) ;
#10468 = ADVANCED_FACE ( 'NONE', ( #19719 ), #11930, .F. ) ;
#10469 = AXIS2_PLACEMENT_3D ( 'NONE', #14603, #1823, #16143 ) ;
#10470 = CARTESIAN_POINT ( 'NONE',  ( -0.8220851292435327196, -62.91215678473957240, 248.9926560891072143 ) ) ;
#10471 = FACE_OUTER_BOUND ( 'NONE', #12125, .T. ) ;
#10472 = EDGE_LOOP ( 'NONE', ( #6234, #16108, #15311 ) ) ;
#10473 = AXIS2_PLACEMENT_3D ( 'NONE', #549, #12914, #6390 ) ;
#10474 = DIRECTION ( 'NONE',  ( 1.000000000000000000, 0.000000000000000000, 0.000000000000000000 ) ) ;
#10475 = LINE ( 'NONE', #10575, #18609 ) ;
#10476 = VERTEX_POINT ( 'NONE', #12141 ) ;
#10477 = CARTESIAN_POINT ( 'NONE',  ( -86.99687941525527890, 106.8407010200819371, -21.44284787283443094 ) ) ;
#10478 = CARTESIAN_POINT ( 'NONE',  ( 7.500000000000008882, 164.0736214083062805, 60.00000000000000000 ) ) ;
#10479 = DIRECTION ( 'NONE',  ( -0.3420201433256694901, 0.9396926207859082059, 0.000000000000000000 ) ) ;
#10480 = CARTESIAN_POINT ( 'NONE',  ( -10.52001906124801778, 3.255534882825997123, 248.9926560891072143 ) ) ;
#10481 = EDGE_CURVE ( 'NONE', #8663, #10934, #8777, .T. ) ;
#10482 = UNCERTAINTY_MEASURE_WITH_UNIT (LENGTH_MEASURE( 1.000000000000000082E-05 ), #20157, 'distance_accuracy_value', 'NONE');
#10483 = CARTESIAN_POINT ( 'NONE',  ( 132.0570769712678043, -87.76803911441056982, 39.72258563631385897 ) ) ;
#10484 = CARTESIAN_POINT ( 'NONE',  ( 0.000000000000000000, 0.000000000000000000, 60.00000000000000000 ) ) ;
#10485 = ORIENTED_EDGE ( 'NONE', *, *, #838, .T. ) ;
#10486 = CARTESIAN_POINT ( 'NONE',  ( -18.92519137117329109, 56.02932139001825362, 248.9926560891072143 ) ) ;
#10487 = VERTEX_POINT ( 'NONE', #10306 ) ;
#10488 = ORIENTED_EDGE ( 'NONE', *, *, #2616, .F. ) ;
#10489 = LINE ( 'NONE', #18486, #15803 ) ;
#10490 = ORIENTED_EDGE ( 'NONE', *, *, #6662, .T. ) ;
#10491 = ORIENTED_EDGE ( 'NONE', *, *, #3641, .F. ) ;
#10492 = EDGE_CURVE ( 'NONE', #13175, #6802, #14971, .T. ) ;
#10493 = EDGE_CURVE ( 'NONE', #11632, #7001, #8973, .T. ) ;
#10494 = EDGE_CURVE ( 'NONE', #11413, #7733, #18194, .T. ) ;
#10495 = CARTESIAN_POINT ( 'NONE',  ( 0.000000000000000000, 0.000000000000000000, 283.5832628385307999 ) ) ;
#10496 = CARTESIAN_POINT ( 'NONE',  ( 166.7850001792985495, -199.9999999999999716, 0.000000000000000000 ) ) ;
#10497 = ORIENTED_EDGE ( 'NONE', *, *, #5534, .T. ) ;
#10498 = CARTESIAN_POINT ( 'NONE',  ( 0.000000000000000000, 0.000000000000000000, 248.9926560891072143 ) ) ;
#10499 = DIRECTION ( 'NONE',  ( 0.000000000000000000, 0.000000000000000000, 1.000000000000000000 ) ) ;
#10500 = ORIENTED_EDGE ( 'NONE', *, *, #17420, .F. ) ;
#10501 = CARTESIAN_POINT ( 'NONE',  ( -131.9327818480801966, -71.37991627326493926, 43.78367249533801697 ) ) ;
#10502 = CARTESIAN_POINT ( 'NONE',  ( -32.62092819947992695, -51.24245927909985454, 293.5832628385307999 ) ) ;
#10503 = CARTESIAN_POINT ( 'NONE',  ( -79.05640494597940915, -127.4758205975444270, 49.99999999999999289 ) ) ;
#10504 = VERTEX_POINT ( 'NONE', #10604 ) ;
#10505 = EDGE_CURVE ( 'NONE', #16088, #9468, #2853, .T. ) ;
#10506 = CIRCLE ( 'NONE', #16741, 7.500000000000012434 ) ;
#10507 = DIRECTION ( 'NONE',  ( 1.000000000000000000, 0.000000000000000000, 0.000000000000000000 ) ) ;
#10508 = CARTESIAN_POINT ( 'NONE',  ( -18.77710619359115896, -55.62246070845775137, 111.4180192758973931 ) ) ;
#10509 = CARTESIAN_POINT ( 'NONE',  ( -75.55085777469670916, 117.8649308618484355, 11.41353043461176142 ) ) ;
#10510 = ORIENTED_EDGE ( 'NONE', *, *, #984, .F. ) ;
#10511 = LINE ( 'NONE', #2963, #7776 ) ;
#10512 = DIRECTION ( 'NONE',  ( 1.000000000000000000, 0.000000000000000000, -0.000000000000000000 ) ) ;
#10513 = ORIENTED_EDGE ( 'NONE', *, *, #2365, .T. ) ;
#10514 = ORIENTED_EDGE ( 'NONE', *, *, #2001, .T. ) ;
#10515 = DIRECTION ( 'NONE',  ( -0.000000000000000000, -0.000000000000000000, -1.000000000000000000 ) ) ;
#10516 = ADVANCED_FACE ( 'NONE', ( #16757 ), #16664, .F. ) ;
#10517 = EDGE_LOOP ( 'NONE', ( #2238, #17549, #9687, #12720 ) ) ;
#10518 = DIRECTION ( 'NONE',  ( -0.000000000000000000, -0.000000000000000000, 1.000000000000000000 ) ) ;
#10519 = LINE ( 'NONE', #5835, #439 ) ;
#10520 = CIRCLE ( 'NONE', #12486, 62.91752772691707207 ) ;
#10521 = EDGE_LOOP ( 'NONE', ( #8764, #77, #18413, #15179 ) ) ;
#10522 = AXIS2_PLACEMENT_3D ( 'NONE', #10631, #16890, #15346 ) ;
#10523 = CARTESIAN_POINT ( 'NONE',  ( 88.24590234222766583, -121.2961002105575972, -4.876953754043664269 ) ) ;
#10524 = CARTESIAN_POINT ( 'NONE',  ( -30.74413178637153976, 54.89456854707572830, 293.5832628385307999 ) ) ;
#10525 = EDGE_CURVE ( 'NONE', #14438, #1213, #18401, .T. ) ;
#10526 = AXIS2_PLACEMENT_3D ( 'NONE', #8808, #13402, #10242 ) ;
#10527 = CARTESIAN_POINT ( 'NONE',  ( -5.281164089014727558, -2.240720816136031690, 293.5832628385307999 ) ) ;
#10528 = CARTESIAN_POINT ( 'NONE',  ( 53.40245231972179596, 28.94983032429848535, 293.5832628385307999 ) ) ;
#10529 = DIRECTION ( 'NONE',  ( 0.000000000000000000, 0.000000000000000000, 1.000000000000000000 ) ) ;
#10530 = CARTESIAN_POINT ( 'NONE',  ( 103.2967819461768073, 53.25886146954521649, 14.88498244535472992 ) ) ;
#10531 = CARTESIAN_POINT ( 'NONE',  ( -3.143238168843667690, 31.03941509555038181, 14.88498244535547599 ) ) ;
#10532 = DIRECTION ( 'NONE',  ( 1.000000000000000000, 0.000000000000000000, 0.000000000000000000 ) ) ;
#10533 = DIRECTION ( 'NONE',  ( 0.3420201433256630508, 0.9396926207859104263, -0.000000000000000000 ) ) ;
#10534 = ORIENTED_EDGE ( 'NONE', *, *, #145, .F. ) ;
#10535 =( BOUNDED_CURVE ( )  B_SPLINE_CURVE ( 3, ( #18245, #666, #4231, #9136 ),
 .UNSPECIFIED., .F., .F. ) 
 B_SPLINE_CURVE_WITH_KNOTS ( ( 4, 4 ),
 ( 1.920639998745670818, 3.141592653589790896 ),
 .UNSPECIFIED. ) 
 CURVE ( )  GEOMETRIC_REPRESENTATION_ITEM ( )  RATIONAL_B_SPLINE_CURVE ( ( 1.000000000000000000, 0.8795833682608498183, 0.8795833682608498183, 1.000000000000000000 ) ) 
 REPRESENTATION_ITEM ( '' )  );
#10536 = CARTESIAN_POINT ( 'NONE',  ( 0.000000000000000000, 0.000000000000000000, 283.5832628385307999 ) ) ;
#10537 = DIRECTION ( 'NONE',  ( -0.000000000000000000, -0.000000000000000000, 1.000000000000000000 ) ) ;
#10538 = VECTOR ( 'NONE', #3296, 1000.000000000000114 ) ;
#10539 = CIRCLE ( 'NONE', #13469, 60.74260934110282051 ) ;
#10540 = ORIENTED_EDGE ( 'NONE', *, *, #3128, .F. ) ;
#10541 = VERTEX_POINT ( 'NONE', #13784 ) ;
#10542 =( NAMED_UNIT ( * ) PLANE_ANGLE_UNIT ( ) SI_UNIT ( $, .RADIAN. ) );
#10543 = AXIS2_PLACEMENT_3D ( 'NONE', #10009, #13067, #17794 ) ;
#10544 = ORIENTED_EDGE ( 'NONE', *, *, #3964, .F. ) ;
#10545 = LINE ( 'NONE', #14136, #5120 ) ;
#10546 = AXIS2_PLACEMENT_3D ( 'NONE', #4926, #6557, #403 ) ;
#10547 = ORIENTED_EDGE ( 'NONE', *, *, #4535, .T. ) ;
#10548 = DIRECTION ( 'NONE',  ( -0.9848077530122092416, 0.1736481776669241694, 0.000000000000000000 ) ) ;
#10549 = DIRECTION ( 'NONE',  ( 0.000000000000000000, 0.000000000000000000, -1.000000000000000000 ) ) ;
#10550 = CYLINDRICAL_SURFACE ( 'NONE', #7422, 106.4288957539801004 ) ;
#10551 = DIRECTION ( 'NONE',  ( 1.000000000000000000, 0.000000000000000000, 0.000000000000000000 ) ) ;
#10552 = AXIS2_PLACEMENT_3D ( 'NONE', #4387, #19934, #7354 ) ;
#10553 = FACE_OUTER_BOUND ( 'NONE', #15706, .T. ) ;
#10554 = DIRECTION ( 'NONE',  ( 1.000000000000000000, 1.613511099790693471E-16, 0.000000000000000000 ) ) ;
#10555 = ORIENTED_EDGE ( 'NONE', *, *, #4589, .T. ) ;
#10556 = CARTESIAN_POINT ( 'NONE',  ( 163.5019688434126977, -20.99123081650019884, 49.99999999999999289 ) ) ;
#10557 = CARTESIAN_POINT ( 'NONE',  ( -134.6900874600844134, -73.16343714252982977, 8.507184036954340556 ) ) ;
#10558 = CARTESIAN_POINT ( 'NONE',  ( 131.9259051260548290, -88.29481989229334715, 0.2208891356029132336 ) ) ;
#10559 = CIRCLE ( 'NONE', #18083, 3.224098631618459443 ) ;
#10560 = CARTESIAN_POINT ( 'NONE',  ( 12.28122767885846400, -61.70726652483821084, 293.5832628385307999 ) ) ;
#10561 = DIRECTION ( 'NONE',  ( 0.000000000000000000, 0.000000000000000000, 1.000000000000000000 ) ) ;
#10562 = DIRECTION ( 'NONE',  ( -0.1736481776669404065, -0.9848077530122062440, 1.238751781085795583E-15 ) ) ;
#10563 = VERTEX_POINT ( 'NONE', #2750 ) ;
#10564 = CARTESIAN_POINT ( 'NONE',  ( 0.000000000000000000, 60.00000000000000000, -105.0000000000000142 ) ) ;
#10565 = AXIS2_PLACEMENT_3D ( 'NONE', #18834, #7970, #3177 ) ;
#10566 = EDGE_LOOP ( 'NONE', ( #11443, #5490, #16527, #4160 ) ) ;
#10567 = ORIENTED_EDGE ( 'NONE', *, *, #17649, .T. ) ;
#10568 = ORIENTED_EDGE ( 'NONE', *, *, #15664, .F. ) ;
#10569 = AXIS2_PLACEMENT_3D ( 'NONE', #14751, #734, #10238 ) ;
#10570 = ADVANCED_FACE ( 'NONE', ( #12247 ), #4378, .T. ) ;
#10571 = DIRECTION ( 'NONE',  ( -0.9271237148521547233, 0.3747554100459928872, 0.000000000000000000 ) ) ;
#10572 = PLANE ( 'NONE',  #595 ) ;
#10573 = ORIENTED_EDGE ( 'NONE', *, *, #9752, .T. ) ;
#10574 = DIRECTION ( 'NONE',  ( 1.000000000000000000, 0.000000000000000000, 0.000000000000000000 ) ) ;
#10575 = CARTESIAN_POINT ( 'NONE',  ( 44.79787735033391272, -41.02212542604627288, 283.5832628385307999 ) ) ;
#10576 = ORIENTED_EDGE ( 'NONE', *, *, #4155, .T. ) ;
#10577 = DIRECTION ( 'NONE',  ( -0.000000000000000000, -0.000000000000000000, 1.000000000000000000 ) ) ;
#10578 = CARTESIAN_POINT ( 'NONE',  ( 156.4179374840099683, -52.02840013023883614, 39.99999999999999289 ) ) ;
#10579 = CARTESIAN_POINT ( 'NONE',  ( 12.24586475280413289, -24.22555452564822787, 39.88498244535536941 ) ) ;
#10580 = PLANE ( 'NONE',  #15725 ) ;
#10581 = EDGE_CURVE ( 'NONE', #2735, #1702, #20030, .T. ) ;
#10582 = EDGE_CURVE ( 'NONE', #17735, #16054, #5195, .T. ) ;
#10583 = CARTESIAN_POINT ( 'NONE',  ( 127.7402033587085555, -78.63140257241676068, 48.47023495424932804 ) ) ;
#10584 = VECTOR ( 'NONE', #2549, 1000.000000000000000 ) ;
#10585 = DIRECTION ( 'NONE',  ( 1.000000000000000000, 3.491481338843133355E-15, -0.000000000000000000 ) ) ;
#10586 = ORIENTED_EDGE ( 'NONE', *, *, #506, .F. ) ;
#10587 = EDGE_CURVE ( 'NONE', #14697, #12460, #17289, .T. ) ;
#10588 = EDGE_LOOP ( 'NONE', ( #14225, #12642 ) ) ;
#10589 = CARTESIAN_POINT ( 'NONE',  ( 0.000000000000000000, 0.000000000000000000, 49.99999999999999289 ) ) ;
#10590 = VERTEX_POINT ( 'NONE', #7647 ) ;
#10591 = VERTEX_POINT ( 'NONE', #3357 ) ;
#10592 = DIRECTION ( 'NONE',  ( 0.000000000000000000, 0.000000000000000000, 1.000000000000000000 ) ) ;
#10593 = ORIENTED_EDGE ( 'NONE', *, *, #11769, .F. ) ;
#10594 = ORIENTED_EDGE ( 'NONE', *, *, #4883, .T. ) ;
#10595 = EDGE_CURVE ( 'NONE', #7405, #19299, #7751, .T. ) ;
#10596 = LINE ( 'NONE', #1408, #2254 ) ;
#10597 = LINE ( 'NONE', #12338, #5169 ) ;
#10598 = VERTEX_POINT ( 'NONE', #12555 ) ;
#10599 = AXIS2_PLACEMENT_3D ( 'NONE', #11227, #6545, #4803 ) ;
#10600 = DIRECTION ( 'NONE',  ( 0.000000000000000000, 0.000000000000000000, -1.000000000000000000 ) ) ;
#10601 = DIRECTION ( 'NONE',  ( -0.8479630283625698706, 0.5300553768524376430, 0.000000000000000000 ) ) ;
#10602 = EDGE_LOOP ( 'NONE', ( #5880, #4905, #1348 ) ) ;
#10603 = CARTESIAN_POINT ( 'NONE',  ( 0.000000000000000000, 10.39230484541327471, -5.498853076140229456E-16 ) ) ;
#10604 = CARTESIAN_POINT ( 'NONE',  ( 148.9554720520395392, -17.67108784863215476, 49.99999999999999289 ) ) ;
#10605 = DIRECTION ( 'NONE',  ( -1.000000000000000000, 0.000000000000000000, 0.000000000000000000 ) ) ;
#10606 = ORIENTED_EDGE ( 'NONE', *, *, #2283, .T. ) ;
#10607 = EDGE_CURVE ( 'NONE', #15125, #18959, #1717, .T. ) ;
#10608 = CARTESIAN_POINT ( 'NONE',  ( 41.02212542604613077, 44.79787735033405482, 283.5832628385307999 ) ) ;
#10609 = EDGE_CURVE ( 'NONE', #2886, #17034, #15737, .T. ) ;
#10610 = CARTESIAN_POINT ( 'NONE',  ( 0.8038475772933615371, 5.196152422706624030, -9.000000000000001776 ) ) ;
#10611 = CIRCLE ( 'NONE', #4757, 62.91752772691707207 ) ;
#10612 = CARTESIAN_POINT ( 'NONE',  ( -62.90240729679781850, -1.379293853801974779, 293.5832628385307999 ) ) ;
#10613 = ORIENTED_EDGE ( 'NONE', *, *, #3022, .T. ) ;
#10614 = ADVANCED_FACE ( 'NONE', ( #12659 ), #18921, .T. ) ;
#10615 = CARTESIAN_POINT ( 'NONE',  ( -50.93469132750304595, -59.42266395395774481, 248.9926560891072143 ) ) ;
#10616 = LINE ( 'NONE', #4596, #4354 ) ;
#10617 = EDGE_LOOP ( 'NONE', ( #19575, #18268, #11605, #8961 ) ) ;
#10618 = ORIENTED_EDGE ( 'NONE', *, *, #7181, .F. ) ;
#10619 = CARTESIAN_POINT ( 'NONE',  ( -97.49999999999997158, -115.4778303846450029, 29.99999999999999289 ) ) ;
#10620 = ORIENTED_EDGE ( 'NONE', *, *, #14791, .F. ) ;
#10621 = AXIS2_PLACEMENT_3D ( 'NONE', #1774, #231, #18973 ) ;
#10622 = EDGE_CURVE ( 'NONE', #17815, #9217, #14095, .T. ) ;
#10623 = DIRECTION ( 'NONE',  ( 6.982962677686266711E-15, -0.000000000000000000, 1.000000000000000000 ) ) ;
#10624 = ORIENTED_EDGE ( 'NONE', *, *, #9346, .F. ) ;
#10625 = STYLED_ITEM ( 'NONE', ( #16067 ), #8201 ) ;
#10626 = CARTESIAN_POINT ( 'NONE',  ( 87.34436178610390300, -121.9468435064317617, -3.953023745371848197 ) ) ;
#10627 = LINE ( 'NONE', #1333, #2774 ) ;
#10628 = LINE ( 'NONE', #11957, #15033 ) ;
#10629 = FACE_OUTER_BOUND ( 'NONE', #13987, .T. ) ;
#10630 =( NAMED_UNIT ( * ) PLANE_ANGLE_UNIT ( ) SI_UNIT ( $, .RADIAN. ) );
#10631 = CARTESIAN_POINT ( 'NONE',  ( 128.2779226595531270, 102.2982297021113141, 39.99999999999999289 ) ) ;
#10632 = ADVANCED_FACE ( 'NONE', ( #17179 ), #3060, .F. ) ;
#10633 = FACE_BOUND ( 'NONE', #8946, .T. ) ;
#10634 = EDGE_CURVE ( 'NONE', #4813, #7427, #5004, .T. ) ;
#10635 = DIRECTION ( 'NONE',  ( -0.000000000000000000, -0.000000000000000000, 1.000000000000000000 ) ) ;
#10636 = ADVANCED_FACE ( 'NONE', ( #1520 ), #15841, .F. ) ;
#10637 = CARTESIAN_POINT ( 'NONE',  ( 97.11506731898820988, -115.6376992562306469, 29.64291924541058521 ) ) ;
#10639 = EDGE_CURVE ( 'NONE', #11211, #6009, #8055, .T. ) ;
#10638 = CIRCLE ( 'NONE', #5763, 9.000000000000000000 ) ;
#10640 = ORIENTED_EDGE ( 'NONE', *, *, #13519, .T. ) ;
#10641 = DIRECTION ( 'NONE',  ( -0.4693298356057531429, 0.8830229359480288309, 0.000000000000000000 ) ) ;
#10642 = CARTESIAN_POINT ( 'NONE',  ( 73.06915264522001507, 28.06281046684300762, 248.9926560891072143 ) ) ;
#10643 = ORIENTED_EDGE ( 'NONE', *, *, #9774, .F. ) ;
#10644 = ADVANCED_FACE ( 'NONE', ( #11023 ), #6541, .T. ) ;
#10646 = EDGE_LOOP ( 'NONE', ( #12756, #2814 ) ) ;
#10645 = AXIS2_PLACEMENT_3D ( 'NONE', #19906, #8953, #1395 ) ;
#10647 = DIRECTION ( 'NONE',  ( 0.000000000000000000, 0.000000000000000000, 1.000000000000000000 ) ) ;
#10648 = EDGE_CURVE ( 'NONE', #7495, #13974, #10406, .T. ) ;
#10649 = ORIENTED_EDGE ( 'NONE', *, *, #10037, .T. ) ;
#10650 = FACE_BOUND ( 'NONE', #4237, .T. ) ;
#10651 = ORIENTED_EDGE ( 'NONE', *, *, #1543, .T. ) ;
#10652 = CARTESIAN_POINT ( 'NONE',  ( 4.189777606611760026E-13, -60.00000000000000000, -115.0000000000000000 ) ) ;
#10653 = VECTOR ( 'NONE', #19115, 999.9999999999998863 ) ;
#10654 = AXIS2_PLACEMENT_3D ( 'NONE', #7289, #17678, #4013 ) ;
#10655 = DIRECTION ( 'NONE',  ( -1.000000000000000000, 0.000000000000000000, 0.000000000000000000 ) ) ;
#10656 = CARTESIAN_POINT ( 'NONE',  ( -37.93579148621510200, -68.46530598706782200, 110.9660488491356887 ) ) ;
#10657 = DIRECTION ( 'NONE',  ( 0.9396926207859104263, 0.3420201433256629953, -6.568644312862836368E-15 ) ) ;
#10658 = CARTESIAN_POINT ( 'NONE',  ( 38.35506425062457225, 44.43084819159290788, 248.9926560891072143 ) ) ;
#10659 = ORIENTED_EDGE ( 'NONE', *, *, #3614, .F. ) ;
#10660 = CARTESIAN_POINT ( 'NONE',  ( -5.524863963826648572, -116.0870680293436408, 39.88498244535549730 ) ) ;
#10661 = CARTESIAN_POINT ( 'NONE',  ( -133.6648977371338844, -68.07564730482667414, 0.2001739272734736064 ) ) ;
#10662 = CIRCLE ( 'NONE', #16551, 112.8770930172170495 ) ;
#10663 = CARTESIAN_POINT ( 'NONE',  ( 133.2381282822229025, -68.90431829399533115, -0.9334320511221024796 ) ) ;
#10664 = PLANE ( 'NONE',  #11777 ) ;
#10665 = LINE ( 'NONE', #6083, #9183 ) ;
#10666 = CARTESIAN_POINT ( 'NONE',  ( -132.1020537416607397, -71.17237643004155245, 36.09957904933038719 ) ) ;
#10667 = EDGE_LOOP ( 'NONE', ( #1223, #7590 ) ) ;
#10668 = CARTESIAN_POINT ( 'NONE',  ( 0.000000000000000000, 0.000000000000000000, 283.5832628385307999 ) ) ;
#10669 = ADVANCED_FACE ( 'NONE', ( #17281 ), #9394, .T. ) ;
#10670 = ORIENTED_EDGE ( 'NONE', *, *, #11613, .T. ) ;
#10671 = ORIENTED_EDGE ( 'NONE', *, *, #16534, .F. ) ;
#10672 = CIRCLE ( 'NONE', #8069, 7.500000000000020428 ) ;
#10673 = CIRCLE ( 'NONE', #11662, 60.74260934110282051 ) ;
#10674 = EDGE_LOOP ( 'NONE', ( #8198, #1539 ) ) ;
#10675 = CARTESIAN_POINT ( 'NONE',  ( -141.5781605588074683, -18.79909027762237272, 20.09932341090167895 ) ) ;
#10676 = CARTESIAN_POINT ( 'NONE',  ( -12.16118437606778535, -23.99289710269258080, 14.88498244535553461 ) ) ;
#10677 = DIRECTION ( 'NONE',  ( -0.000000000000000000, 1.000000000000000000, -0.000000000000000000 ) ) ;
#10678 = ORIENTED_EDGE ( 'NONE', *, *, #8774, .F. ) ;
#10679 = CARTESIAN_POINT ( 'NONE',  ( -139.3225548399015850, -10.84875705434604498, -14.11339856648029212 ) ) ;
#10680 = DIRECTION ( 'NONE',  ( 0.9993852124581887875, -0.03505990758545544927, 0.000000000000000000 ) ) ;
#10681 = ORIENTED_EDGE ( 'NONE', *, *, #4004, .T. ) ;
#10682 = CARTESIAN_POINT ( 'NONE',  ( -85.01747478753389942, 109.2823643868091779, -19.52988736366387101 ) ) ;
#10683 = DIRECTION ( 'NONE',  ( 0.000000000000000000, 0.000000000000000000, -1.000000000000000000 ) ) ;
#10684 = FACE_OUTER_BOUND ( 'NONE', #14708, .T. ) ;
#10685 = CARTESIAN_POINT ( 'NONE',  ( 0.1482032042127255644, 2.204400401860219905, 9.000000000000001776 ) ) ;
#10686 = CARTESIAN_POINT ( 'NONE',  ( 57.55901709132171362, 11.54977938102105028, 132.4711112102474146 ) ) ;
#10687 = VECTOR ( 'NONE', #19591, 1000.000000000000000 ) ;
#10688 = AXIS2_PLACEMENT_3D ( 'NONE', #7347, #19825, #15325 ) ;
#10689 = AXIS2_PLACEMENT_3D ( 'NONE', #8438, #9974, #2008 ) ;
#10690 = CARTESIAN_POINT ( 'NONE',  ( 129.1041139275565968, -76.37100075998219495, 47.39509621162856945 ) ) ;
#10691 = FACE_OUTER_BOUND ( 'NONE', #10247, .T. ) ;
#10692 = EDGE_LOOP ( 'NONE', ( #5958, #14907, #3387 ) ) ;
#10693 = EDGE_CURVE ( 'NONE', #6419, #11868, #6237, .T. ) ;
#10694 = ORIENTED_EDGE ( 'NONE', *, *, #4334, .F. ) ;
#10695 = CARTESIAN_POINT ( 'NONE',  ( 152.4599531637113330, -36.50981547336952104, 49.99999999999999289 ) ) ;
#10696 = ORIENTED_EDGE ( 'NONE', *, *, #3411, .F. ) ;
#10697 = ORIENTED_EDGE ( 'NONE', *, *, #17308, .T. ) ;
#10698 = DIRECTION ( 'NONE',  ( 1.000000000000000000, 0.000000000000000000, 0.000000000000000000 ) ) ;
#10699 = ORIENTED_EDGE ( 'NONE', *, *, #16004, .F. ) ;
#10700 = CARTESIAN_POINT ( 'NONE',  ( -159.9599531637108782, -36.50981547337168109, 49.99999999999999289 ) ) ;
#10701 = VECTOR ( 'NONE', #11902, 1000.000000000000000 ) ;
#10702 = CARTESIAN_POINT ( 'NONE',  ( -1.140219284730587620E-14, -7.573738413550444193, 4.881900264494501762 ) ) ;
#10703 = AXIS2_PLACEMENT_3D ( 'NONE', #16402, #19469, #11680 ) ;
#10704 = EDGE_CURVE ( 'NONE', #1551, #6246, #9453, .T. ) ;
#10705 = FACE_OUTER_BOUND ( 'NONE', #4560, .T. ) ;
#10706 = DIRECTION ( 'NONE',  ( 0.000000000000000000, 1.000000000000000000, 0.000000000000000000 ) ) ;
#10707 = ORIENTED_EDGE ( 'NONE', *, *, #8387, .T. ) ;
#10708 = CARTESIAN_POINT ( 'NONE',  ( 0.01899995639453595439, 7.352259170992715198, -5.265513565426385156 ) ) ;
#10709 = CARTESIAN_POINT ( 'NONE',  ( 2.244911526960062012E-13, -1.379293853801755176, 248.9926560891072143 ) ) ;
#10710 = EDGE_LOOP ( 'NONE', ( #12553, #3468, #16818, #13618 ) ) ;
#10711 = DIRECTION ( 'NONE',  ( 0.000000000000000000, 0.000000000000000000, -1.000000000000000000 ) ) ;
#10712 = DIRECTION ( 'NONE',  ( 0.000000000000000000, 0.000000000000000000, 1.000000000000000000 ) ) ;
#10713 = CARTESIAN_POINT ( 'NONE',  ( -50.93469132750304595, -59.42266395395774481, 110.7293897666001214 ) ) ;
#10714 = VECTOR ( 'NONE', #8963, 1000.000000000000000 ) ;
#10715 = DIRECTION ( 'NONE',  ( 0.000000000000000000, 1.000000000000000000, 0.000000000000000000 ) ) ;
#10716 = CARTESIAN_POINT ( 'NONE',  ( 8.833100819207578169, 58.03804081968171147, 112.0427633081292953 ) ) ;
#10717 = DIRECTION ( 'NONE',  ( 1.000000000000000000, 0.000000000000000000, 0.000000000000000000 ) ) ;
#10718 = VECTOR ( 'NONE', #947, 1000.000000000000000 ) ;
#10719 = AXIS2_PLACEMENT_3D ( 'NONE', #20077, #9338, #3481 ) ;
#10720 = ORIENTED_EDGE ( 'NONE', *, *, #9514, .F. ) ;
#10721 = EDGE_CURVE ( 'NONE', #16961, #739, #15428, .T. ) ;
#10722 = AXIS2_PLACEMENT_3D ( 'NONE', #6961, #11940, #13181 ) ;
#10723 = CARTESIAN_POINT ( 'NONE',  ( 0.000000000000000000, 0.000000000000000000, -115.0000000000000142 ) ) ;
#10724 = CARTESIAN_POINT ( 'NONE',  ( 49.67518383744835120, -60.47951622432768204, 132.4711112102474146 ) ) ;
#10725 = ORIENTED_EDGE ( 'NONE', *, *, #19006, .F. ) ;
#10726 = EDGE_LOOP ( 'NONE', ( #9142, #14781, #560 ) ) ;
#10727 = DIRECTION ( 'NONE',  ( 0.3088643371590157338, -0.9511061040868794558, 0.000000000000000000 ) ) ;
#10728 = VERTEX_POINT ( 'NONE', #6439 ) ;
#10729 = CARTESIAN_POINT ( 'NONE',  ( -146.5157903719973262, 32.27091178421088102, -11.39721689603033283 ) ) ;
#10730 = EDGE_CURVE ( 'NONE', #18597, #12303, #15982, .T. ) ;
#10731 = CARTESIAN_POINT ( 'NONE',  ( -3.453261854573022482, -4.581103194069998885, 293.5832628385307999 ) ) ;
#10732 = ORIENTED_EDGE ( 'NONE', *, *, #16609, .F. ) ;
#10733 = CARTESIAN_POINT ( 'NONE',  ( 84.44661573609288041, -123.9709896190459233, 0.1742278272254467741 ) ) ;
#10734 = CARTESIAN_POINT ( 'NONE',  ( 32.50000000000000000, 0.000000000000000000, -115.0000000000000000 ) ) ;
#10735 = AXIS2_PLACEMENT_3D ( 'NONE', #16836, #8949, #17982 ) ;
#10736 = AXIS2_PLACEMENT_3D ( 'NONE', #12858, #5101, #11431 ) ;
#10737 = EDGE_CURVE ( 'NONE', #5703, #13232, #2584, .T. ) ;
#10738 = FACE_OUTER_BOUND ( 'NONE', #3801, .T. ) ;
#10739 = DIRECTION ( 'NONE',  ( -0.7430374143461878633, 0.6692498792541777819, 0.000000000000000000 ) ) ;
#10740 = ORIENTED_EDGE ( 'NONE', *, *, #16251, .T. ) ;
#10741 = CARTESIAN_POINT ( 'NONE',  ( 7.950000000000000178, 10.39230484541327471, 0.000000000000000000 ) ) ;
#10742 = DIRECTION ( 'NONE',  ( 0.000000000000000000, 0.000000000000000000, -1.000000000000000000 ) ) ;
#10743 = CARTESIAN_POINT ( 'NONE',  ( 1.378965026025638009E-14, 26.82911281104372847, 39.88498244535545467 ) ) ;
#10744 = CARTESIAN_POINT ( 'NONE',  ( 97.93656923779383305, -133.3799209237882053, 32.92832214187814799 ) ) ;
#10745 = ORIENTED_EDGE ( 'NONE', *, *, #8520, .F. ) ;
#10746 = CIRCLE ( 'NONE', #7171, 150.0000000000000284 ) ;
#10747 = EDGE_CURVE ( 'NONE', #55, #10158, #19506, .T. ) ;
#10748 = CARTESIAN_POINT ( 'NONE',  ( 156.4179374840099683, -52.02840013023883614, 60.00000000000000000 ) ) ;
#10749 = CARTESIAN_POINT ( 'NONE',  ( -25.47058595421603044, -74.01264520835145788, 111.4180192758973931 ) ) ;
#10750 = VERTEX_POINT ( 'NONE', #3752 ) ;
#10751 = VECTOR ( 'NONE', #10230, 1000.000000000000114 ) ;
#10752 = AXIS2_PLACEMENT_3D ( 'NONE', #3057, #6332, #18603 ) ;
#10753 = EDGE_LOOP ( 'NONE', ( #11133, #11727, #3574, #4468 ) ) ;
#10754 = DIRECTION ( 'NONE',  ( 1.000000000000000000, 0.000000000000000000, 0.000000000000000000 ) ) ;
#10755 = ORIENTED_EDGE ( 'NONE', *, *, #7850, .T. ) ;
#10756 = CARTESIAN_POINT ( 'NONE',  ( 51.24245927909996112, -32.62092819947974220, 283.5832628385307999 ) ) ;
#10757 = FACE_BOUND ( 'NONE', #14856, .T. ) ;
#10758 = EDGE_LOOP ( 'NONE', ( #9909, #8789 ) ) ;
#10759 = EDGE_CURVE ( 'NONE', #10176, #13146, #14798, .T. ) ;
#10760 = DIRECTION ( 'NONE',  ( 0.000000000000000000, 0.000000000000000000, 1.000000000000000000 ) ) ;
#10761 = DIRECTION ( 'NONE',  ( -0.000000000000000000, -1.000000000000000000, -0.000000000000000000 ) ) ;
#10762 = ADVANCED_FACE ( 'NONE', ( #19217 ), #15943, .T. ) ;
#10763 = DIRECTION ( 'NONE',  ( 0.8660254037844380415, 0.5000000000000009992, 0.000000000000000000 ) ) ;
#10764 = CARTESIAN_POINT ( 'NONE',  ( -99.98863955314961061, -130.5690324404936291, 36.60999800948973615 ) ) ;
#10765 = CARTESIAN_POINT ( 'NONE',  ( -167.4599531637108782, -36.50981547337168109, 49.99999999999999289 ) ) ;
#10766 = VECTOR ( 'NONE', #5020, 1000.000000000000000 ) ;
#10767 = AXIS2_PLACEMENT_3D ( 'NONE', #8923, #18047, #3824 ) ;
#10768 = FACE_OUTER_BOUND ( 'NONE', #889, .T. ) ;
#10769 = CARTESIAN_POINT ( 'NONE',  ( -134.5315346870343376, -74.37329574990532421, 6.387021999321605747 ) ) ;
#10770 = CARTESIAN_POINT ( 'NONE',  ( 132.7564094051595589, -84.67399327755590832, 0.8739656915399692805 ) ) ;
#10771 = DIRECTION ( 'NONE',  ( -0.8660254037844415942, 0.4999999999999950040, 0.000000000000000000 ) ) ;
#10772 = DIRECTION ( 'NONE',  ( -0.4999999999999888978, -0.8660254037844449249, 0.000000000000000000 ) ) ;
#10773 = CARTESIAN_POINT ( 'NONE',  ( -125.5405970674900971, -82.09774788367874976, 49.55822172878893639 ) ) ;
#10774 = ORIENTED_EDGE ( 'NONE', *, *, #7850, .F. ) ;
#10775 = EDGE_CURVE ( 'NONE', #10444, #7454, #585, .T. ) ;
#10776 = PRODUCT_DEFINITION_SHAPE ( 'NONE', 'NONE',  #20251 ) ;
#10777 = CYLINDRICAL_SURFACE ( 'NONE', #15758, 32.50000000000000000 ) ;
#10778 = VERTEX_POINT ( 'NONE', #9793 ) ;
#10779 = CIRCLE ( 'NONE', #979, 3.224098631618460331 ) ;
#10780 = VERTEX_POINT ( 'NONE', #19317 ) ;
#10781 = ORIENTED_EDGE ( 'NONE', *, *, #12363, .F. ) ;
#10782 = ADVANCED_FACE ( 'NONE', ( #5205 ), #1929, .T. ) ;
#10783 = PLANE ( 'NONE',  #10233 ) ;
#10784 = DIRECTION ( 'NONE',  ( -0.000000000000000000, 0.000000000000000000, 1.000000000000000000 ) ) ;
#10785 = CARTESIAN_POINT ( 'NONE',  ( 0.000000000000000000, 0.000000000000000000, 83.57543755549745867 ) ) ;
#10786 = ORIENTED_EDGE ( 'NONE', *, *, #12166, .T. ) ;
#10787 = CARTESIAN_POINT ( 'NONE',  ( 0.000000000000000000, 0.000000000000000000, 40.00000000000000000 ) ) ;
#10788 = CARTESIAN_POINT ( 'NONE',  ( 61.70726652483817531, 12.28122767885865763, 248.9926560891072143 ) ) ;
#10789 = EDGE_CURVE ( 'NONE', #3700, #3934, #17305, .T. ) ;
#10790 = ORIENTED_EDGE ( 'NONE', *, *, #17948, .F. ) ;
#10791 = CARTESIAN_POINT ( 'NONE',  ( -82.42673853863954037, 112.2670201977909556, -16.56329132253156189 ) ) ;
#10792 = CARTESIAN_POINT ( 'NONE',  ( -97.49999999999997158, -190.0000000000000000, 30.00000000000000000 ) ) ;
#10793 = LINE ( 'NONE', #9265, #11404 ) ;
#10794 = CARTESIAN_POINT ( 'NONE',  ( 0.000000000000000000, 0.000000000000000000, 293.5832628385307999 ) ) ;
#10795 = CARTESIAN_POINT ( 'NONE',  ( 71.18887634719571622, -147.8252249328912740, 49.99999999999999289 ) ) ;
#10796 = DIRECTION ( 'NONE',  ( 0.000000000000000000, 0.000000000000000000, -1.000000000000000000 ) ) ;
#10797 = ORIENTED_EDGE ( 'NONE', *, *, #19603, .F. ) ;
#10798 = ORIENTED_EDGE ( 'NONE', *, *, #15405, .F. ) ;
#10799 = ORIENTED_EDGE ( 'NONE', *, *, #9852, .T. ) ;
#10800 = ORIENTED_EDGE ( 'NONE', *, *, #3663, .F. ) ;
#10801 = DIRECTION ( 'NONE',  ( -0.1736481776669340227, 0.9848077530122073542, 0.000000000000000000 ) ) ;
#10802 = CIRCLE ( 'NONE', #1334, 110.0000000000000142 ) ;
#10803 = ORIENTED_EDGE ( 'NONE', *, *, #14231, .F. ) ;
#10804 = EDGE_LOOP ( 'NONE', ( #7306, #17209, #4085, #9989 ) ) ;
#10805 = AXIS2_PLACEMENT_3D ( 'NONE', #3417, #17232, #9552 ) ;
#10806 = CARTESIAN_POINT ( 'NONE',  ( 0.000000000000000000, 0.000000000000000000, 83.57543755549745867 ) ) ;
#10807 = CARTESIAN_POINT ( 'NONE',  ( -110.0000000000000142, 285.0000000000000568, 5.000000000000000888 ) ) ;
#10808 = CYLINDRICAL_SURFACE ( 'NONE', #6141, 9.999999999999994671 ) ;
#10809 = ORIENTED_EDGE ( 'NONE', *, *, #15652, .T. ) ;
#10810 = CARTESIAN_POINT ( 'NONE',  ( 37.78198917157319414, -47.56244194535177172, 283.5832628385307999 ) ) ;
#10811 = CARTESIAN_POINT ( 'NONE',  ( 0.000000000000000000, 0.000000000000000000, -10.00000000000000178 ) ) ;
#10812 = ORIENTED_EDGE ( 'NONE', *, *, #6161, .F. ) ;
#10813 = AXIS2_PLACEMENT_3D ( 'NONE', #15697, #14153, #17641 ) ;
#10814 = LINE ( 'NONE', #1416, #3803 ) ;
#10815 = DIRECTION ( 'NONE',  ( 0.000000000000000000, 1.000000000000000000, 0.000000000000000000 ) ) ;
#10816 = CARTESIAN_POINT ( 'NONE',  ( 7.350000000000001421, -3.004629197474319640E-15, -9.000000000000001776 ) ) ;
#10817 = AXIS2_PLACEMENT_3D ( 'NONE', #12662, #19748, #11125 ) ;
#10818 = DIRECTION ( 'NONE',  ( -0.000000000000000000, -1.000000000000000000, -0.000000000000000000 ) ) ;
#10819 = CARTESIAN_POINT ( 'NONE',  ( 3.453261854573465683, 4.581103194070611728, 283.5832628385307999 ) ) ;
#10820 = CARTESIAN_POINT ( 'NONE',  ( -98.89944939536758284, 99.14269198534090322, 38.28897304660228684 ) ) ;
#10821 = ORIENTED_EDGE ( 'NONE', *, *, #17432, .T. ) ;
#10822 = DIRECTION ( 'NONE',  ( 1.047444401652940007E-14, -1.000000000000000000, 0.000000000000000000 ) ) ;
#10823 = ORIENTED_EDGE ( 'NONE', *, *, #3986, .F. ) ;
#10824 = VERTEX_POINT ( 'NONE', #9896 ) ;
#10825 = CARTESIAN_POINT ( 'NONE',  ( -82.80829968035172328, -125.0716697069619840, 35.88848305379081438 ) ) ;
#10826 = ORIENTED_EDGE ( 'NONE', *, *, #438, .T. ) ;
#10827 = CARTESIAN_POINT ( 'NONE',  ( -129.5808341847080669, 64.44470624890260524, -29.94181153629256542 ) ) ;
#10828 = LINE ( 'NONE', #4499, #4034 ) ;
#10829 = ORIENTED_EDGE ( 'NONE', *, *, #18017, .T. ) ;
#10830 = CARTESIAN_POINT ( 'NONE',  ( 96.67521566530152199, -115.8170149452160018, 10.31811481433898692 ) ) ;
#10831 = CARTESIAN_POINT ( 'NONE',  ( -19.74955734591987522, 8.656064874776506102, 248.9926560891072143 ) ) ;
#10832 = EDGE_CURVE ( 'NONE', #599, #9011, #19413, .T. ) ;
#10833 = CIRCLE ( 'NONE', #10184, 7.500000000000003553 ) ;
#10834 = LINE ( 'NONE', #10941, #16686 ) ;
#10835 = EDGE_CURVE ( 'NONE', #16647, #16902, #16629, .T. ) ;
#10836 = FACE_BOUND ( 'NONE', #4488, .T. ) ;
#10837 = EDGE_LOOP ( 'NONE', ( #8295, #10215 ) ) ;
#10838 = DIRECTION ( 'NONE',  ( 6.982962677686266711E-15, -0.000000000000000000, 1.000000000000000000 ) ) ;
#10839 = CARTESIAN_POINT ( 'NONE',  ( 4.189777606611760026E-13, -60.00000000000000000, -100.0000000000000000 ) ) ;
#10840 = ADVANCED_FACE ( 'NONE', ( #11715 ), #16343, .F. ) ;
#10841 = CARTESIAN_POINT ( 'NONE',  ( -32.03743494504725930, 36.03492788066173347, 248.9926560891072143 ) ) ;
#10842 = CARTESIAN_POINT ( 'NONE',  ( 99.15855529360270282, -131.7281685730150400, 35.51823119121745265 ) ) ;
#10843 = ORIENTED_EDGE ( 'NONE', *, *, #3104, .F. ) ;
#10844 = EDGE_CURVE ( 'NONE', #5911, #13255, #17943, .T. ) ;
#10845 = DIRECTION ( 'NONE',  ( 0.000000000000000000, 0.000000000000000000, 1.000000000000000000 ) ) ;
#10846 = LINE ( 'NONE', #17101, #17747 ) ;
#10847 = ADVANCED_FACE ( 'NONE', ( #6932 ), #8558, .F. ) ;
#10848 = ORIENTED_EDGE ( 'NONE', *, *, #18801, .F. ) ;
#10849 = ORIENTED_EDGE ( 'NONE', *, *, #2547, .F. ) ;
#10850 = EDGE_CURVE ( 'NONE', #7403, #7735, #9100, .T. ) ;
#10851 = ORIENTED_EDGE ( 'NONE', *, *, #14893, .T. ) ;
#10852 = DIRECTION ( 'NONE',  ( 0.000000000000000000, 0.000000000000000000, 1.000000000000000000 ) ) ;
#10853 = VECTOR ( 'NONE', #4826, 1000.000000000000114 ) ;
#10854 = EDGE_LOOP ( 'NONE', ( #13661, #12227, #2662, #3794 ) ) ;
#10855 = PLANE ( 'NONE',  #12725 ) ;
#10856 = DIRECTION ( 'NONE',  ( 0.000000000000000000, 0.000000000000000000, -1.000000000000000000 ) ) ;
#10857 = ORIENTED_EDGE ( 'NONE', *, *, #1094, .T. ) ;
#10858 = AXIS2_PLACEMENT_3D ( 'NONE', #13606, #10435, #19852 ) ;
#10859 = DIRECTION ( 'NONE',  ( -0.8830229359480288309, -0.4693298356057531984, 0.000000000000000000 ) ) ;
#10860 = LINE ( 'NONE', #17223, #6681 ) ;
#10861 = DIRECTION ( 'NONE',  ( 0.000000000000000000, 0.000000000000000000, 1.000000000000000000 ) ) ;
#10862 = EDGE_CURVE ( 'NONE', #17330, #5317, #3458, .T. ) ;
#10863 = CARTESIAN_POINT ( 'NONE',  ( -100.6915138157995386, -129.5610470606159481, 37.32613602704453371 ) ) ;
#10864 = LINE ( 'NONE', #17228, #16545 ) ;
#10865 = DIRECTION ( 'NONE',  ( 1.000000000000000000, 0.000000000000000000, 0.000000000000000000 ) ) ;
#10866 = DIRECTION ( 'NONE',  ( 1.000000000000000000, 0.000000000000000000, 0.000000000000000000 ) ) ;
#10867 = DIRECTION ( 'NONE',  ( 0.4693298356057564180, -0.8830229359480272766, 0.000000000000000000 ) ) ;
#10868 = CARTESIAN_POINT ( 'NONE',  ( 128.1750136849898354, -77.98139142652387079, -0.5590989923425794261 ) ) ;
#10869 = VECTOR ( 'NONE', #17003, 1000.000000000000000 ) ;
#10870 = AXIS2_PLACEMENT_3D ( 'NONE', #9883, #16133, #17869 ) ;
#10871 = DIRECTION ( 'NONE',  ( 0.9009688679024154823, 0.4338837391175657809, 0.000000000000000000 ) ) ;
#10872 = DIRECTION ( 'NONE',  ( -0.000000000000000000, 1.000000000000000000, -0.000000000000000000 ) ) ;
#10873 = CARTESIAN_POINT ( 'NONE',  ( -133.2381282822229025, -68.90431829399531694, 40.93343205112707750 ) ) ;
#10874 = VERTEX_POINT ( 'NONE', #6638 ) ;
#10875 = CARTESIAN_POINT ( 'NONE',  ( -0.8220851292435327196, -78.26059000578311498, 132.4711112102474146 ) ) ;
#10876 = ADVANCED_FACE ( 'NONE', ( #3660 ), #19116, .F. ) ;
#10877 = VECTOR ( 'NONE', #1913, 1000.000000000000227 ) ;
#10878 = ADVANCED_FACE ( 'NONE', ( #6733 ), #5104, .F. ) ;
#10879 = VERTEX_POINT ( 'NONE', #13444 ) ;
#10880 = ORIENTED_EDGE ( 'NONE', *, *, #14749, .F. ) ;
#10881 = VECTOR ( 'NONE', #14002, 1000.000000000000114 ) ;
#10882 = EDGE_LOOP ( 'NONE', ( #10694, #16179, #15161, #12939 ) ) ;
#10883 = EDGE_CURVE ( 'NONE', #1562, #6720, #4728, .T. ) ;
#10884 = CARTESIAN_POINT ( 'NONE',  ( -130.9868171408399462, -91.88282611735539263, 0.000000000000000000 ) ) ;
#10885 = CARTESIAN_POINT ( 'NONE',  ( 0.8220851292435327196, 78.26059000578311498, 132.4711112102474146 ) ) ;
#10886 = ORIENTED_EDGE ( 'NONE', *, *, #19259, .F. ) ;
#10887 = CIRCLE ( 'NONE', #771, 15.91767397667354444 ) ;
#10888 = LINE ( 'NONE', #17145, #19164 ) ;
#10889 = DIRECTION ( 'NONE',  ( -0.7430374143461878633, 0.6692498792541777819, 0.000000000000000000 ) ) ;
#10890 = DIRECTION ( 'NONE',  ( 0.000000000000000000, 0.000000000000000000, 1.000000000000000000 ) ) ;
#10891 = CARTESIAN_POINT ( 'NONE',  ( 0.000000000000000000, 0.000000000000000000, 283.5832628385307999 ) ) ;
#10892 = CARTESIAN_POINT ( 'NONE',  ( -1.396592535537253342E-14, 0.000000000000000000, 39.88498244535545467 ) ) ;
#10893 = AXIS2_PLACEMENT_3D ( 'NONE', #15631, #9588, #6430 ) ;
#10894 = CARTESIAN_POINT ( 'NONE',  ( 0.8220851292435327196, 62.91215678473957240, 293.5832628385307999 ) ) ;
#10895 = DIRECTION ( 'NONE',  ( -0.7071067811865493491, 0.000000000000000000, -0.7071067811865455743 ) ) ;
#10896 = ADVANCED_FACE ( 'NONE', ( #5796 ), #13348, .T. ) ;
#10897 = CARTESIAN_POINT ( 'NONE',  ( 131.7825524766324463, -71.64958008132042266, 43.99896812349997077 ) ) ;
#10898 = CARTESIAN_POINT ( 'NONE',  ( -107.4999999999999716, -200.0000000000000000, 0.000000000000000000 ) ) ;
#10899 = EDGE_CURVE ( 'NONE', #16122, #3485, #19902, .T. ) ;
#10900 = VERTEX_POINT ( 'NONE', #18074 ) ;
#10901 = ORIENTED_EDGE ( 'NONE', *, *, #14008, .T. ) ;
#10902 = ORIENTED_EDGE ( 'NONE', *, *, #10899, .F. ) ;
#10903 = VECTOR ( 'NONE', #14042, 1000.000000000000000 ) ;
#10904 = EDGE_CURVE ( 'NONE', #13329, #8156, #4052, .T. ) ;
#10905 = VERTEX_POINT ( 'NONE', #4252 ) ;
#10906 = DIRECTION ( 'NONE',  ( -0.1736481776669273613, 0.9848077530122086864, 1.212578743696387931E-15 ) ) ;
#10907 = VECTOR ( 'NONE', #18570, 999.9999999999998863 ) ;
#10908 = VERTEX_POINT ( 'NONE', #1071 ) ;
#10909 = LINE ( 'NONE', #20223, #16228 ) ;
#10910 = CARTESIAN_POINT ( 'NONE',  ( 41.02350267428969488, 44.79940644582669051, 283.5832628385307999 ) ) ;
#10911 = DIRECTION ( 'NONE',  ( 1.000000000000000000, 0.000000000000000000, -0.000000000000000000 ) ) ;
#10912 = FACE_OUTER_BOUND ( 'NONE', #3144, .T. ) ;
#10913 = CARTESIAN_POINT ( 'NONE',  ( -5.524863963826648572, -116.0870680293436408, 39.88498244535549730 ) ) ;
#10914 = EDGE_LOOP ( 'NONE', ( #13363, #843, #16823, #8440 ) ) ;
#10915 = DIRECTION ( 'NONE',  ( 0.4338837391175643932, -0.9009688679024161484, 0.000000000000000000 ) ) ;
#10916 = DIRECTION ( 'NONE',  ( -0.1736481776669306920, 0.9848077530122080203, 0.000000000000000000 ) ) ;
#10917 = ORIENTED_EDGE ( 'NONE', *, *, #9774, .T. ) ;
#10918 = PRODUCT_DEFINITION_CONTEXT ( 'detailed design', #18620, 'design' ) ;
#10919 = DIRECTION ( 'NONE',  ( -0.9271237148521547233, 0.3747554100459928872, 0.000000000000000000 ) ) ;
#10920 = DIRECTION ( 'NONE',  ( 0.9396926207859114255, -0.3420201433256601642, 0.000000000000000000 ) ) ;
#10921 = AXIS2_PLACEMENT_3D ( 'NONE', #7979, #19142, #412 ) ;
#10922 = DIRECTION ( 'NONE',  ( -0.000000000000000000, -0.000000000000000000, -1.000000000000000000 ) ) ;
#10923 = AXIS2_PLACEMENT_3D ( 'NONE', #16513, #2799, #10655 ) ;
#10924 = DIRECTION ( 'NONE',  ( 0.4999999999999916178, -0.8660254037844435926, -4.304393070272782536E-15 ) ) ;
#10925 = CARTESIAN_POINT ( 'NONE',  ( -10.11498556985118924, 62.09913334491134407, 248.9926560891072143 ) ) ;
#10926 = CARTESIAN_POINT ( 'NONE',  ( -75.12965072324909954, 118.1335604146951113, 8.039948435259535842 ) ) ;
#10927 = ORIENTED_EDGE ( 'NONE', *, *, #17779, .T. ) ;
#10928 = FACE_OUTER_BOUND ( 'NONE', #19347, .T. ) ;
#10929 = ORIENTED_EDGE ( 'NONE', *, *, #11626, .T. ) ;
#10930 = AXIS2_PLACEMENT_3D ( 'NONE', #1672, #8002, #17437 ) ;
#10931 = VERTEX_POINT ( 'NONE', #16734 ) ;
#10932 = CARTESIAN_POINT ( 'NONE',  ( -23.22718332831480481, -56.12853591711337486, 293.5832628385307999 ) ) ;
#10933 = CIRCLE ( 'NONE', #2132, 62.91752772691707207 ) ;
#10934 = VERTEX_POINT ( 'NONE', #2723 ) ;
#10935 = DIRECTION ( 'NONE',  ( 0.000000000000000000, 0.000000000000000000, 1.000000000000000000 ) ) ;
#10936 = DIRECTION ( 'NONE',  ( 1.000000000000000000, 0.000000000000000000, 0.000000000000000000 ) ) ;
#10937 = VERTEX_POINT ( 'NONE', #10579 ) ;
#10938 = CARTESIAN_POINT ( 'NONE',  ( 97.21757233051022240, -115.5955488200751518, 10.33714169725774212 ) ) ;
#10939 = DIRECTION ( 'NONE',  ( 1.000000000000000000, 0.000000000000000000, -0.000000000000000000 ) ) ;
#10940 = PRODUCT_DEFINITION_SHAPE ( 'NONE', 'NONE',  #3524 ) ;
#10941 = CARTESIAN_POINT ( 'NONE',  ( 39.84224160888901167, 67.36461649554546227, 110.9660488491356887 ) ) ;
#10942 = CARTESIAN_POINT ( 'NONE',  ( 45.46865632508072963, -40.28046525994365368, 283.5832628385307999 ) ) ;
#10943 = ORIENTED_EDGE ( 'NONE', *, *, #14231, .T. ) ;
#10944 = CARTESIAN_POINT ( 'NONE',  ( 0.000000000000000000, 0.000000000000000000, -115.0000000000000000 ) ) ;
#10945 = CIRCLE ( 'NONE', #504, 106.4288957539801146 ) ;
#10946 = CARTESIAN_POINT ( 'NONE',  ( -15.91767397667355510, 149.1530343478547422, 60.00000000000000000 ) ) ;
#10947 = CYLINDRICAL_SURFACE ( 'NONE', #12206, 62.91752772691707207 ) ;
#10948 = CARTESIAN_POINT ( 'NONE',  ( 83.54968581051038257, -124.5775662629409766, 37.91678146420370155 ) ) ;
#10949 = ORIENTED_EDGE ( 'NONE', *, *, #17298, .F. ) ;
#10950 = CARTESIAN_POINT ( 'NONE',  ( 78.26059000578310076, 1.379293853802574077, 248.9926560891072143 ) ) ;
#10951 = CARTESIAN_POINT ( 'NONE',  ( 0.000000000000000000, 0.000000000000000000, 283.5832628385307999 ) ) ;
#10952 = ORIENTED_EDGE ( 'NONE', *, *, #6756, .T. ) ;
#10953 = EDGE_CURVE ( 'NONE', #13849, #5317, #2909, .T. ) ;
#10954 = ORIENTED_EDGE ( 'NONE', *, *, #605, .T. ) ;
#10955 = VERTEX_POINT ( 'NONE', #19599 ) ;
#10956 = DIRECTION ( 'NONE',  ( -1.000000000000000000, 0.000000000000000000, 1.047444401652940007E-14 ) ) ;
#10957 = VERTEX_POINT ( 'NONE', #15193 ) ;
#10958 = CARTESIAN_POINT ( 'NONE',  ( -101.1753893487742033, -128.8598102521084456, 2.230270385704167246 ) ) ;
#10959 = B_SPLINE_CURVE_WITH_KNOTS ( 'NONE', 3,
 ( #9827, #6470, #8292, #2068, #115, #19149, #7886, #12797, #18956, #5041, #14233, #9629, #1661, #4942, #14127, #6368, #213, #17319, #12585, #12692, #1964, #12995, #12895, #18848, #8193, #19253, #11157, #17422, #4835, #17621, #317, #15674, #527, #1857, #11055, #9533, #15771, #1754, #6771, #5239, #7987, #3396, #15977, #3693, #3596, #11464 ),
 .UNSPECIFIED., .F., .F.,
 ( 4, 2, 2, 2, 2, 2, 2, 2, 2, 2, 2, 2, 2, 2, 2, 2, 2, 2, 2, 2, 2, 2, 4 ),
 ( 1.214306433183764966E-17, 0.005452065557044396583, 0.01090413111408878102, 0.01363016389261097021, 0.01635619667113315939, 0.02180826222817754123, 0.02317127861743863843, 0.02453429500669972868, 0.02726032778522194389, 0.03271239334226637430, 0.03543842612078860338, 0.03816445889931082552, 0.04361652445635528369, 0.04634255723487753359, 0.04906859001339978349, 0.05452065557044430411, 0.05997272112748881778, 0.06269875390601106768, 0.06542478668453331758, 0.07632891779862233106, 0.07905495057714460871, 0.08178098335566688637, 0.08723304891271140005 ),
 .UNSPECIFIED. ) ;
#10960 = LINE ( 'NONE', #12288, #18172 ) ;
#10961 = ORIENTED_EDGE ( 'NONE', *, *, #7900, .T. ) ;
#10962 = LINE ( 'NONE', #4845, #5989 ) ;
#10963 = DIRECTION ( 'NONE',  ( -1.000000000000000000, 0.000000000000000000, 6.977185866873309606E-15 ) ) ;
#10964 = CARTESIAN_POINT ( 'NONE',  ( -1.629937663769596368, -60.72279549541552512, 283.5832628385307999 ) ) ;
#10965 = ADVANCED_FACE ( 'NONE', ( #5590 ), #1174, .F. ) ;
#10966 = CARTESIAN_POINT ( 'NONE',  ( -99.35210738963753840, -131.4612102079657916, 35.80770037246424664 ) ) ;
#10967 = CARTESIAN_POINT ( 'NONE',  ( -15.91767397667354800, 164.0736214083062805, 49.99999999999999289 ) ) ;
#10968 = VECTOR ( 'NONE', #953, 1000.000000000000000 ) ;
#10969 = EDGE_CURVE ( 'NONE', #4491, #9076, #20000, .T. ) ;
#10970 = CARTESIAN_POINT ( 'NONE',  ( -134.6566615416656418, 38.49973993374615588, 29.87962448166155127 ) ) ;
#10971 = PLANE ( 'NONE',  #14236 ) ;
#10972 = CARTESIAN_POINT ( 'NONE',  ( 12.23146955673593794, 77.31114765718498916, 132.4711112102474146 ) ) ;
#10973 = CARTESIAN_POINT ( 'NONE',  ( -87.50000000000000000, -133.9542832461881687, 30.00000000000000000 ) ) ;
#10974 = CARTESIAN_POINT ( 'NONE',  ( 7.950000000000000178, -5.196152422706636465, -8.999999999999998224 ) ) ;
#10975 = CARTESIAN_POINT ( 'NONE',  ( -130.5436973595314498, -73.98181611797480173, 38.74509961212098830 ) ) ;
#10976 = ORIENTED_EDGE ( 'NONE', *, *, #6559, .T. ) ;
#10977 = CIRCLE ( 'NONE', #11932, 15.91767397667354089 ) ;
#10978 = DIRECTION ( 'NONE',  ( 0.9396926207859068736, 0.3420201433256725987, 0.000000000000000000 ) ) ;
#10979 = EDGE_CURVE ( 'NONE', #9227, #2560, #3950, .T. ) ;
#10980 = VERTEX_POINT ( 'NONE', #7130 ) ;
#10981 = AXIS2_PLACEMENT_3D ( 'NONE', #10787, #20098, #9260 ) ;
#10982 = VERTEX_POINT ( 'NONE', #16543 ) ;
#10983 = VERTEX_POINT ( 'NONE', #2521 ) ;
#10984 = CARTESIAN_POINT ( 'NONE',  ( -142.9809548150034573, -16.70024071994362203, -6.750090680848771285 ) ) ;
#10985 = AXIS2_PLACEMENT_3D ( 'NONE', #6936, #19422, #5403 ) ;
#10986 = CARTESIAN_POINT ( 'NONE',  ( -18.28503710798546678, 57.92514141135458772, 283.5832628385307999 ) ) ;
#10987 = ADVANCED_FACE ( 'NONE', ( #8753 ), #14994, .T. ) ;
#10988 = CARTESIAN_POINT ( 'NONE',  ( -51.77076963420845601, 31.77187437101486367, 283.5832628385307999 ) ) ;
#10989 = CARTESIAN_POINT ( 'NONE',  ( 0.000000000000000000, 0.000000000000000000, -105.0000000000000142 ) ) ;
#10990 = EDGE_CURVE ( 'NONE', #5660, #15236, #19569, .T. ) ;
#10991 = DIRECTION ( 'NONE',  ( 6.982962677686266711E-15, -0.000000000000000000, 1.000000000000000000 ) ) ;
#10992 = DIRECTION ( 'NONE',  ( -0.3747554100459928317, -0.9271237148521548344, 0.000000000000000000 ) ) ;
#10993 = DIRECTION ( 'NONE',  ( -0.000000000000000000, -0.000000000000000000, 1.000000000000000000 ) ) ;
#10994 = CARTESIAN_POINT ( 'NONE',  ( -159.9599531637108782, -36.50981547337168109, 49.99999999999999289 ) ) ;
#10995 = AXIS2_PLACEMENT_3D ( 'NONE', #11807, #7129, #16342 ) ;
#10996 = ORIENTED_EDGE ( 'NONE', *, *, #5021, .T. ) ;
#10997 = VECTOR ( 'NONE', #723, 999.9999999999998863 ) ;
#10998 = CARTESIAN_POINT ( 'NONE',  ( 134.5985778548171652, -73.87143572891014287, 32.93474295113719563 ) ) ;
#10999 = CARTESIAN_POINT ( 'NONE',  ( 134.7188131032333445, -72.93593548660992099, 30.49611318099233515 ) ) ;
#11000 = ORIENTED_EDGE ( 'NONE', *, *, #13031, .F. ) ;
#11002 = ORIENTED_EDGE ( 'NONE', *, *, #19983, .F. ) ;
#11001 = CIRCLE ( 'NONE', #19508, 60.74260934110282051 ) ;
#11003 = ADVANCED_FACE ( 'NONE', ( #257 ), #6409, .T. ) ;
#11004 = ORIENTED_EDGE ( 'NONE', *, *, #13108, .T. ) ;
#11005 = VERTEX_POINT ( 'NONE', #3332 ) ;
#11006 = CYLINDRICAL_SURFACE ( 'NONE', #14476, 62.91752772691707207 ) ;
#11007 = VERTEX_POINT ( 'NONE', #3231 ) ;
#11008 = DIRECTION ( 'NONE',  ( 0.000000000000000000, 0.000000000000000000, 1.000000000000000000 ) ) ;
#11009 = DIRECTION ( 'NONE',  ( 0.000000000000000000, 0.000000000000000000, 1.000000000000000000 ) ) ;
#11010 = FACE_BOUND ( 'NONE', #17803, .T. ) ;
#11011 = SURFACE_STYLE_FILL_AREA ( #1922 ) ;
#11012 = DIRECTION ( 'NONE',  ( -0.000000000000000000, -0.000000000000000000, -1.000000000000000000 ) ) ;
#11013 = VERTEX_POINT ( 'NONE', #13962 ) ;
#11014 = ADVANCED_FACE ( 'NONE', ( #14178 ), #1278, .T. ) ;
#11015 = CARTESIAN_POINT ( 'NONE',  ( 131.0911649403506374, -72.90709374210200622, -5.085999411194714881 ) ) ;
#11016 = CARTESIAN_POINT ( 'NONE',  ( 0.000000000000000000, 0.000000000000000000, 60.00000000000000000 ) ) ;
#11017 = EDGE_CURVE ( 'NONE', #2887, #182, #7924, .T. ) ;
#11018 = ORIENTED_EDGE ( 'NONE', *, *, #5787, .F. ) ;
#11019 = ADVANCED_FACE ( 'NONE', ( #2930 ), #9471, .T. ) ;
#11020 = AXIS2_PLACEMENT_3D ( 'NONE', #13059, #12960, #11627 ) ;
#11021 = AXIS2_PLACEMENT_3D ( 'NONE', #162, #4128, #7105 ) ;
#11022 = CARTESIAN_POINT ( 'NONE',  ( -86.93963912163985697, 117.1591715488320062, -27.74534354785872736 ) ) ;
#11023 = FACE_OUTER_BOUND ( 'NONE', #17968, .T. ) ;
#11024 = PLANE ( 'NONE',  #11277 ) ;
#11025 = DIRECTION ( 'NONE',  ( -0.000000000000000000, -0.000000000000000000, 1.000000000000000000 ) ) ;
#11026 = LINE ( 'NONE', #16051, #18981 ) ;
#11027 = PLANE ( 'NONE',  #10323 ) ;
#11028 = EDGE_LOOP ( 'NONE', ( #4190, #13022, #5087, #9993 ) ) ;
#11029 = CARTESIAN_POINT ( 'NONE',  ( 176.1792632384392334, -186.5724904703758682, 30.00000000000000000 ) ) ;
#11030 = EDGE_CURVE ( 'NONE', #9508, #15527, #10793, .T. ) ;
#11031 = EDGE_LOOP ( 'NONE', ( #10671, #3273, #18087, #5676 ) ) ;
#11032 = VECTOR ( 'NONE', #1619, 1000.000000000000000 ) ;
#11033 = VERTEX_POINT ( 'NONE', #12428 ) ;
#11034 = DIRECTION ( 'NONE',  ( -0.000000000000000000, -0.000000000000000000, -1.000000000000000000 ) ) ;
#11035 = AXIS2_PLACEMENT_3D ( 'NONE', #4005, #11968, #10153 ) ;
#11036 = VERTEX_POINT ( 'NONE', #15508 ) ;
#11037 = CARTESIAN_POINT ( 'NONE',  ( -134.7839606304467566, 57.38400188359436527, -26.41417060242037351 ) ) ;
#11038 = DIRECTION ( 'NONE',  ( 1.000000000000000000, 0.000000000000000000, -0.000000000000000000 ) ) ;
#11039 = ORIENTED_EDGE ( 'NONE', *, *, #13054, .F. ) ;
#11040 = EDGE_CURVE ( 'NONE', #4473, #5793, #7722, .T. ) ;
#11041 = CARTESIAN_POINT ( 'NONE',  ( 97.50000000000000000, -133.9542832461881687, 9.999999999999996447 ) ) ;
#11042 = DIRECTION ( 'NONE',  ( 0.000000000000000000, 0.000000000000000000, 1.000000000000000000 ) ) ;
#11043 = VECTOR ( 'NONE', #12421, 1000.000000000000000 ) ;
#11044 = ADVANCED_FACE ( 'NONE', ( #14070 ), #20207, .T. ) ;
#11045 = DIRECTION ( 'NONE',  ( -0.000000000000000000, -0.000000000000000000, -1.000000000000000000 ) ) ;
#11046 = AXIS2_PLACEMENT_3D ( 'NONE', #9719, #17206, #14123 ) ;
#11047 = CIRCLE ( 'NONE', #2892, 60.74260934110282051 ) ;
#11048 = VERTEX_POINT ( 'NONE', #3033 ) ;
#11049 = CARTESIAN_POINT ( 'NONE',  ( -110.0000000000000142, 275.0000000000000000, -67.49999999999997158 ) ) ;
#11050 = DIRECTION ( 'NONE',  ( 0.2225209339563183342, -0.9749279121818226201, 0.000000000000000000 ) ) ;
#11051 = CARTESIAN_POINT ( 'NONE',  ( 127.4413876050234364, 0.000000000000000000, 39.88498244535456649 ) ) ;
#11052 = FACE_OUTER_BOUND ( 'NONE', #14575, .T. ) ;
#11053 = VERTEX_POINT ( 'NONE', #18788 ) ;
#11054 = CARTESIAN_POINT ( 'NONE',  ( -8.833100819207983179, -58.03804081968163331, 132.4711112102474146 ) ) ;
#11055 = CARTESIAN_POINT ( 'NONE',  ( -91.62566160141871308, 118.7664292046248278, 40.53793933303452945 ) ) ;
#11056 = EDGE_LOOP ( 'NONE', ( #13506, #16129 ) ) ;
#11057 = EDGE_LOOP ( 'NONE', ( #11468, #5470, #17465, #11117, #5604 ) ) ;
#11058 = EDGE_LOOP ( 'NONE', ( #18307, #17672, #11314, #4570 ) ) ;
#11059 = DIRECTION ( 'NONE',  ( 0.000000000000000000, -1.000000000000000000, 0.000000000000000000 ) ) ;
#11060 = AXIS2_PLACEMENT_3D ( 'NONE', #15629, #6429, #1617 ) ;
#11061 = VECTOR ( 'NONE', #13624, 1000.000000000000227 ) ;
#11062 = ORIENTED_EDGE ( 'NONE', *, *, #18300, .F. ) ;
#11063 = AXIS2_PLACEMENT_3D ( 'NONE', #13681, #16567, #5716 ) ;
#11064 = CARTESIAN_POINT ( 'NONE',  ( -98.02151343901456926, -133.2674925500989218, 6.780480114272203984 ) ) ;
#11065 = CARTESIAN_POINT ( 'NONE',  ( -26.04958516073518382, 47.87779272208825176, 248.9926560891072143 ) ) ;
#11066 = EDGE_LOOP ( 'NONE', ( #16243, #15824, #9245, #3142 ) ) ;
#11067 = DIRECTION ( 'NONE',  ( 0.000000000000000000, 0.000000000000000000, 1.000000000000000000 ) ) ;
#11068 = CARTESIAN_POINT ( 'NONE',  ( 0.000000000000000000, 0.000000000000000000, 293.5832628385307999 ) ) ;
#11069 = CARTESIAN_POINT ( 'NONE',  ( -97.49999999944088813, -115.4778303847294154, 10.15726746729510310 ) ) ;
#11070 = CARTESIAN_POINT ( 'NONE',  ( -95.49511753037597828, -115.9200926448052940, 33.43441907682297654 ) ) ;
#11071 = LINE ( 'NONE', #17119, #16857 ) ;
#11072 = DIRECTION ( 'NONE',  ( -0.9396926207859057634, -0.3420201433256757073, 0.000000000000000000 ) ) ;
#11073 = FACE_BOUND ( 'NONE', #17398, .T. ) ;
#11074 = DIRECTION ( 'NONE',  ( 0.000000000000000000, 1.000000000000000000, 0.000000000000000000 ) ) ;
#11075 = DIRECTION ( 'NONE',  ( -0.000000000000000000, -0.000000000000000000, -1.000000000000000000 ) ) ;
#11076 = DIRECTION ( 'NONE',  ( 0.000000000000000000, 0.000000000000000000, 1.000000000000000000 ) ) ;
#11077 = AXIS2_PLACEMENT_3D ( 'NONE', #385, #16142, #13245 ) ;
#11078 = CARTESIAN_POINT ( 'NONE',  ( -126.7459963399414988, -80.26907437897514797, 41.00725567157765283 ) ) ;
#11079 = CIRCLE ( 'NONE', #12372, 99.99999999999997158 ) ;
#11080 = ORIENTED_EDGE ( 'NONE', *, *, #3017, .T. ) ;
#11081 = CARTESIAN_POINT ( 'NONE',  ( 38.41834839689379777, -68.18670162478817076, 132.4711112102474146 ) ) ;
#11082 = ORIENTED_EDGE ( 'NONE', *, *, #15894, .T. ) ;
#11083 = ORIENTED_EDGE ( 'NONE', *, *, #14050, .T. ) ;
#11084 = VERTEX_POINT ( 'NONE', #9365 ) ;
#11085 = AXIS2_PLACEMENT_3D ( 'NONE', #19837, #5834, #13286 ) ;
#11086 = CARTESIAN_POINT ( 'NONE',  ( -145.0141832565074935, -14.10286991559387459, 4.805853499333125889 ) ) ;
#11087 = VECTOR ( 'NONE', #2000, 1000.000000000000000 ) ;
#11088 = FACE_OUTER_BOUND ( 'NONE', #20175, .T. ) ;
#11089 = DIRECTION ( 'NONE',  ( 1.000000000000000000, 0.000000000000000000, 0.000000000000000000 ) ) ;
#11090 = CARTESIAN_POINT ( 'NONE',  ( 0.000000000000000000, 0.000000000000000000, 293.5832628385307999 ) ) ;
#11091 = EDGE_CURVE ( 'NONE', #19300, #3549, #15815, .T. ) ;
#11092 = ORIENTED_EDGE ( 'NONE', *, *, #5603, .F. ) ;
#11093 = CARTESIAN_POINT ( 'NONE',  ( -44.43084819159250287, 38.35506425062501989, 248.9926560891072143 ) ) ;
#11094 = DIRECTION ( 'NONE',  ( 0.000000000000000000, 0.000000000000000000, 1.000000000000000000 ) ) ;
#11095 = CARTESIAN_POINT ( 'NONE',  ( 128.2779226595531270, 102.2982297021113141, 49.99999999999999289 ) ) ;
#11096 = CARTESIAN_POINT ( 'NONE',  ( 97.63534213009857865, -133.7771032679719667, 31.65634370844862389 ) ) ;
#11097 = LINE ( 'NONE', #9869, #11676 ) ;
#11098 = ORIENTED_EDGE ( 'NONE', *, *, #4298, .F. ) ;
#11099 = CARTESIAN_POINT ( 'NONE',  ( 134.7130977013151778, -72.98159303036058532, 30.74846602018423170 ) ) ;
#11100 = TOROIDAL_SURFACE ( 'NONE', #9493, 160.0000000000000284, 10.00000000000000000 ) ;
#11101 = FACE_OUTER_BOUND ( 'NONE', #19224, .T. ) ;
#11102 = ORIENTED_EDGE ( 'NONE', *, *, #10990, .T. ) ;
#11103 = EDGE_LOOP ( 'NONE', ( #17472, #17317, #7213, #13925 ) ) ;
#11104 = EDGE_CURVE ( 'NONE', #8290, #12020, #949, .T. ) ;
#11105 = ORIENTED_EDGE ( 'NONE', *, *, #16479, .F. ) ;
#11106 = EDGE_CURVE ( 'NONE', #5457, #16596, #1294, .T. ) ;
#11107 = ORIENTED_EDGE ( 'NONE', *, *, #1932, .T. ) ;
#11108 = ADVANCED_FACE ( 'NONE', ( #10684 ), #16942, .T. ) ;
#11109 = DIRECTION ( 'NONE',  ( 1.000000000000000000, 0.000000000000000000, 0.000000000000000000 ) ) ;
#11110 = EDGE_LOOP ( 'NONE', ( #8171, #3154, #19936 ) ) ;
#11111 = DIRECTION ( 'NONE',  ( -1.000000000000000000, -0.000000000000000000, -0.000000000000000000 ) ) ;
#11112 = CARTESIAN_POINT ( 'NONE',  ( -101.4288913641181438, -128.4806265586112204, 37.95194130168881230 ) ) ;
#11113 = VECTOR ( 'NONE', #5328, 1000.000000000000000 ) ;
#11114 = SURFACE_SIDE_STYLE ('',( #11011 ) ) ;
#11115 = EDGE_CURVE ( 'NONE', #15357, #108, #5352, .T. ) ;
#11116 = DIRECTION ( 'NONE',  ( 6.982962677686266711E-15, -0.000000000000000000, 1.000000000000000000 ) ) ;
#11117 = ORIENTED_EDGE ( 'NONE', *, *, #4376, .T. ) ;
#11118 = AXIS2_PLACEMENT_3D ( 'NONE', #13911, #20156, #19747 ) ;
#11119 = DIRECTION ( 'NONE',  ( -0.5000000000000039968, 0.8660254037844363761, 0.000000000000000000 ) ) ;
#11120 = CARTESIAN_POINT ( 'NONE',  ( 0.000000000000000000, 0.000000000000000000, 132.4711112102474146 ) ) ;
#11121 = ADVANCED_FACE ( 'NONE', ( #18472 ), #1388, .F. ) ;
#11122 = VERTEX_POINT ( 'NONE', #6102 ) ;
#11123 = DIRECTION ( 'NONE',  ( 1.000000000000000000, 0.000000000000000000, 0.000000000000000000 ) ) ;
#11124 = DIRECTION ( 'NONE',  ( -0.3420201433256602197, -0.9396926207859115365, 0.000000000000000000 ) ) ;
#11125 = DIRECTION ( 'NONE',  ( 1.000000000000000000, 0.000000000000000000, 0.000000000000000000 ) ) ;
#11126 = CARTESIAN_POINT ( 'NONE',  ( 0.000000000000000000, 0.000000000000000000, 269.6944534026102360 ) ) ;
#11127 = CARTESIAN_POINT ( 'NONE',  ( 50.93469132750264095, 59.42266395395811429, 132.4711112102474146 ) ) ;
#11128 = CYLINDRICAL_SURFACE ( 'NONE', #16025, 7.500000000000007105 ) ;
#11129 = CARTESIAN_POINT ( 'NONE',  ( 0.000000000000000000, 164.0736214083062805, 60.00000000000000000 ) ) ;
#11130 = EDGE_LOOP ( 'NONE', ( #5024, #11018, #10274, #10421 ) ) ;
#11131 = AXIS2_PLACEMENT_3D ( 'NONE', #9897, #690, #586 ) ;
#11132 = FACE_OUTER_BOUND ( 'NONE', #2695, .T. ) ;
#11133 = ORIENTED_EDGE ( 'NONE', *, *, #10361, .F. ) ;
#11134 = ADVANCED_FACE ( 'NONE', ( #6311 ), #9770, .T. ) ;
#11135 = VECTOR ( 'NONE', #7158, 1000.000000000000000 ) ;
#11136 = ORIENTED_EDGE ( 'NONE', *, *, #10493, .T. ) ;
#11137 = ADVANCED_FACE ( 'NONE', ( #356, #9866 ), #567, .T. ) ;
#11138 = FACE_OUTER_BOUND ( 'NONE', #4950, .T. ) ;
#11139 = ORIENTED_EDGE ( 'NONE', *, *, #10124, .T. ) ;
#11140 = CARTESIAN_POINT ( 'NONE',  ( -137.5420331966829224, 53.19132841792027477, -24.01216543166409068 ) ) ;
#11141 = DIRECTION ( 'NONE',  ( -6.982962677686266711E-15, 0.000000000000000000, -1.000000000000000000 ) ) ;
#11142 = VERTEX_POINT ( 'NONE', #16221 ) ;
#11143 = DIRECTION ( 'NONE',  ( 1.000000000000000000, 0.000000000000000000, 0.000000000000000000 ) ) ;
#11144 = LINE ( 'NONE', #15475, #2993 ) ;
#11145 = VECTOR ( 'NONE', #14938, 1000.000000000000114 ) ;
#11146 = EDGE_CURVE ( 'NONE', #15308, #18601, #12933, .T. ) ;
#11147 = VECTOR ( 'NONE', #16919, 1000.000000000000000 ) ;
#11148 = DIRECTION ( 'NONE',  ( -0.7660444431189835646, 0.6427876096865328126, 0.000000000000000000 ) ) ;
#11149 = DIRECTION ( 'NONE',  ( -0.000000000000000000, -0.000000000000000000, 1.000000000000000000 ) ) ;
#11150 = ORIENTED_EDGE ( 'NONE', *, *, #9209, .F. ) ;
#11151 = DIRECTION ( 'NONE',  ( 0.7660444431189792347, -0.6427876096865379196, 0.000000000000000000 ) ) ;
#11152 = DIRECTION ( 'NONE',  ( -0.000000000000000000, -0.000000000000000000, 1.000000000000000000 ) ) ;
#11153 = CARTESIAN_POINT ( 'NONE',  ( -159.9599531637108782, -36.50981547337168109, 60.00000000000000000 ) ) ;
#11154 = CARTESIAN_POINT ( 'NONE',  ( 97.52847697650780390, -113.9950050384823896, 37.53234943820369551 ) ) ;
#11155 = ORIENTED_EDGE ( 'NONE', *, *, #15866, .F. ) ;
#11156 = LINE ( 'NONE', #9826, #5826 ) ;
#11157 = CARTESIAN_POINT ( 'NONE',  ( -80.29253715427383042, 126.7026982456581123, 31.79868549975239134 ) ) ;
#11158 = EDGE_CURVE ( 'NONE', #5962, #5133, #15917, .T. ) ;
#11159 = ORIENTED_EDGE ( 'NONE', *, *, #15739, .T. ) ;
#11160 = VERTEX_POINT ( 'NONE', #11197 ) ;
#11161 = ORIENTED_EDGE ( 'NONE', *, *, #1099, .T. ) ;
#11162 = CONTEXT_DEPENDENT_SHAPE_REPRESENTATION ( #20042, #10776 ) ;
#11163 = ORIENTED_EDGE ( 'NONE', *, *, #18932, .T. ) ;
#11164 = EDGE_CURVE ( 'NONE', #9389, #9422, #8436, .T. ) ;
#11165 = CARTESIAN_POINT ( 'NONE',  ( -97.53517841124883603, -133.9083944458743076, 9.039724941871954300 ) ) ;
#11166 = CARTESIAN_POINT ( 'NONE',  ( -45.84586732611835913, 36.66871011346426457, 132.4711112102474146 ) ) ;
#11167 = ORIENTED_EDGE ( 'NONE', *, *, #705, .F. ) ;
#11168 = EDGE_CURVE ( 'NONE', #14479, #4599, #5182, .T. ) ;
#11169 = CIRCLE ( 'NONE', #8566, 106.4288957539801430 ) ;
#11170 = LINE ( 'NONE', #328, #19075 ) ;
#11171 = DIRECTION ( 'NONE',  ( 0.000000000000000000, 0.000000000000000000, 1.000000000000000000 ) ) ;
#11172 = CARTESIAN_POINT ( 'NONE',  ( 62.18629025319814474, -9.564549117045299198, 293.5832628385307999 ) ) ;
#11173 = CARTESIAN_POINT ( 'NONE',  ( -95.47048624632753899, -116.1260213179369600, 31.97844772384138068 ) ) ;
#11174 = CARTESIAN_POINT ( 'NONE',  ( 5.281164089014827923, 2.240720816136096083, 283.5832628385307999 ) ) ;
#11175 = DIRECTION ( 'NONE',  ( 0.4999999999999950040, 0.8660254037844415942, 0.000000000000000000 ) ) ;
#11176 = FACE_OUTER_BOUND ( 'NONE', #12816, .T. ) ;
#11177 = CARTESIAN_POINT ( 'NONE',  ( 38.35506425062457225, 44.43084819159290788, 110.7293897666001214 ) ) ;
#11178 = CARTESIAN_POINT ( 'NONE',  ( -136.4994460260997187, -31.11111111111111782, -115.0000000000000142 ) ) ;
#11179 = CARTESIAN_POINT ( 'NONE',  ( 0.000000000000000000, 0.000000000000000000, 293.5832628385307999 ) ) ;
#11180 = VERTEX_POINT ( 'NONE', #2105 ) ;
#11181 = DIRECTION ( 'NONE',  ( -0.000000000000000000, -0.000000000000000000, 1.000000000000000000 ) ) ;
#11182 = CIRCLE ( 'NONE', #18365, 3.224098631618460331 ) ;
#11183 = VECTOR ( 'NONE', #17851, 1000.000000000000114 ) ;
#11184 = VERTEX_POINT ( 'NONE', #11305 ) ;
#11185 = CIRCLE ( 'NONE', #2372, 106.4288957539801004 ) ;
#11186 = ORIENTED_EDGE ( 'NONE', *, *, #5772, .T. ) ;
#11187 = CIRCLE ( 'NONE', #420, 7.500000000000007105 ) ;
#11188 = ORIENTED_EDGE ( 'NONE', *, *, #13518, .T. ) ;
#11189 = CARTESIAN_POINT ( 'NONE',  ( -143.0918807612787020, -16.54827070355140961, 16.43686625575313087 ) ) ;
#11190 = DIRECTION ( 'NONE',  ( -0.7660444431189770143, 0.6427876096865404731, 5.346191897317644801E-15 ) ) ;
#11191 = VECTOR ( 'NONE', #5356, 1000.000000000000000 ) ;
#11192 = PLANE ( 'NONE',  #6813 ) ;
#11193 = AXIS2_PLACEMENT_3D ( 'NONE', #17832, #15048, #2878 ) ;
#11194 = DIRECTION ( 'NONE',  ( -0.000000000000000000, -0.000000000000000000, 1.000000000000000000 ) ) ;
#11195 = LINE ( 'NONE', #3532, #3228 ) ;
#11196 = CARTESIAN_POINT ( 'NONE',  ( 163.5019688434126977, -20.99123081650019884, 60.00000000000000000 ) ) ;
#11197 = CARTESIAN_POINT ( 'NONE',  ( -147.0809924354783220, 29.44794838685322702, -9.999999999999978684 ) ) ;
#11198 = CIRCLE ( 'NONE', #15451, 62.91752772691707207 ) ;
#11199 = FACE_OUTER_BOUND ( 'NONE', #16550, .T. ) ;
#11200 = CARTESIAN_POINT ( 'NONE',  ( 4.189777606611760026E-13, -60.00000000000000000, -100.0000000000000000 ) ) ;
#11201 = VERTEX_POINT ( 'NONE', #17461 ) ;
#11202 = CARTESIAN_POINT ( 'NONE',  ( 134.7264294273387009, -65.94569739564036581, 35.17155507723151686 ) ) ;
#11203 = DIRECTION ( 'NONE',  ( -0.9993852124581887875, 0.03505990758545545621, 0.000000000000000000 ) ) ;
#11204 = ORIENTED_EDGE ( 'NONE', *, *, #13216, .F. ) ;
#11205 = VECTOR ( 'NONE', #2040, 1000.000000000000000 ) ;
#11206 = AXIS2_PLACEMENT_3D ( 'NONE', #7020, #14591, #14787 ) ;
#11207 = ORIENTED_EDGE ( 'NONE', *, *, #20167, .F. ) ;
#11208 = ORIENTED_EDGE ( 'NONE', *, *, #9603, .T. ) ;
#11209 = EDGE_CURVE ( 'NONE', #17841, #19703, #16020, .T. ) ;
#11210 = DIRECTION ( 'NONE',  ( 0.03505990758545895342, 0.9993852124581886764, 0.000000000000000000 ) ) ;
#11211 = VERTEX_POINT ( 'NONE', #3730 ) ;
#11212 = CARTESIAN_POINT ( 'NONE',  ( -11.54977938102048007, 57.55901709132182731, 112.0427633081291816 ) ) ;
#11213 = AXIS2_PLACEMENT_3D ( 'NONE', #16127, #2118, #19305 ) ;
#11214 = PLANE ( 'NONE',  #1400 ) ;
#11215 = FACE_OUTER_BOUND ( 'NONE', #17553, .T. ) ;
#11216 = CARTESIAN_POINT ( 'NONE',  ( 50.37374754117451658, -141.2886604036503115, 39.99999999999999289 ) ) ;
#11217 = ORIENTED_EDGE ( 'NONE', *, *, #6244, .F. ) ;
#11218 = CARTESIAN_POINT ( 'NONE',  ( 130.1901167961280237, -74.50443780700841501, -6.262183608668058454 ) ) ;
#11219 = CARTESIAN_POINT ( 'NONE',  ( 3.123743752084413128, -4.811834253409454476, 283.5832628385307999 ) ) ;
#11220 = ORIENTED_EDGE ( 'NONE', *, *, #7890, .T. ) ;
#11221 = EDGE_CURVE ( 'NONE', #10541, #1274, #12833, .T. ) ;
#11222 = CARTESIAN_POINT ( 'NONE',  ( -4.196299268919082337, -3.911853314815666671, 293.5832628385307999 ) ) ;
#11224 = CIRCLE ( 'NONE', #5042, 42.50000000000000000 ) ;
#11223 = CARTESIAN_POINT ( 'NONE',  ( 0.000000000000000000, 0.000000000000000000, 132.4711112102474146 ) ) ;
#11225 = CARTESIAN_POINT ( 'NONE',  ( -49.67518383744793908, 60.47951622432801599, 248.9926560891072143 ) ) ;
#11226 = ADVANCED_FACE ( 'NONE', ( #19092 ), #16117, .T. ) ;
#11227 = CARTESIAN_POINT ( 'NONE',  ( -36.66871011346412246, -45.84586732611848703, 110.7293897666001214 ) ) ;
#11228 = DIRECTION ( 'NONE',  ( 0.03505990758545895342, 0.9993852124581886764, 0.000000000000000000 ) ) ;
#11229 = VECTOR ( 'NONE', #11858, 1000.000000000000000 ) ;
#11230 = CARTESIAN_POINT ( 'NONE',  ( -54.07248341783231638, 32.16802499836798290, 248.9926560891072143 ) ) ;
#11231 = CARTESIAN_POINT ( 'NONE',  ( 84.30790708731538530, -124.0658650269852501, 39.57734081243646074 ) ) ;
#11232 = VERTEX_POINT ( 'NONE', #17563 ) ;
#11233 = DIRECTION ( 'NONE',  ( -0.000000000000000000, -0.000000000000000000, -1.000000000000000000 ) ) ;
#11234 = AXIS2_PLACEMENT_3D ( 'NONE', #19917, #12238, #15525 ) ;
#11235 = EDGE_LOOP ( 'NONE', ( #2745, #5990, #4945, #9170 ) ) ;
#11236 = VERTEX_POINT ( 'NONE', #2208 ) ;
#11237 = ADVANCED_FACE ( 'NONE', ( #11502 ), #665, .T. ) ;
#11238 = FACE_OUTER_BOUND ( 'NONE', #16158, .T. ) ;
#11239 = ORIENTED_EDGE ( 'NONE', *, *, #8592, .F. ) ;
#11240 = CARTESIAN_POINT ( 'NONE',  ( -49.59485801383857506, -102.5175491340983882, 14.88498244535579929 ) ) ;
#11241 = CARTESIAN_POINT ( 'NONE',  ( -29.99999999999887379, 275.0000000000000000, 12.49999999999916511 ) ) ;
#11242 = ORIENTED_EDGE ( 'NONE', *, *, #7383, .T. ) ;
#11243 = MECHANICAL_DESIGN_GEOMETRIC_PRESENTATION_REPRESENTATION (  '', ( #19433 ), #1113 ) ;
#11244 = CARTESIAN_POINT ( 'NONE',  ( 32.50000000000000000, 3.980102097228897837E-15, -40.00000000000000000 ) ) ;
#11245 = CARTESIAN_POINT ( 'NONE',  ( 17.50000000000001776, 0.000000000000000000, 49.99999999999998579 ) ) ;
#11246 = EDGE_CURVE ( 'NONE', #19595, #10224, #3895, .T. ) ;
#11247 = AXIS2_PLACEMENT_3D ( 'NONE', #17656, #10161, #2201 ) ;
#11248 = DIRECTION ( 'NONE',  ( 6.982962677686266711E-15, -0.000000000000000000, 1.000000000000000000 ) ) ;
#11249 = ADVANCED_FACE ( 'NONE', ( #6711 ), #6911, .F. ) ;
#11250 = EDGE_CURVE ( 'NONE', #12652, #15683, #1951, .T. ) ;
#11251 = CARTESIAN_POINT ( 'NONE',  ( 7.350000000000001421, 7.794228634059941818, 4.500000000000007994 ) ) ;
#11252 = CARTESIAN_POINT ( 'NONE',  ( 0.000000000000000000, 0.000000000000000000, 248.9926560891072143 ) ) ;
#11253 = EDGE_LOOP ( 'NONE', ( #1606, #19828, #452 ) ) ;
#11254 = FACE_OUTER_BOUND ( 'NONE', #2116, .T. ) ;
#11255 = CARTESIAN_POINT ( 'NONE',  ( -12.23146955673647795, -77.31114765718486126, 248.9926560891072143 ) ) ;
#11256 = CARTESIAN_POINT ( 'NONE',  ( -109.9999999999874376, 73.61623156955475622, -29.99999999999998579 ) ) ;
#11257 = CARTESIAN_POINT ( 'NONE',  ( 56.84754764479240663, -154.7316448359447634, 39.99999999999999289 ) ) ;
#11258 = VERTEX_POINT ( 'NONE', #9438 ) ;
#11259 = DIRECTION ( 'NONE',  ( 0.000000000000000000, 0.000000000000000000, 1.000000000000000000 ) ) ;
#11260 = DIRECTION ( 'NONE',  ( -0.000000000000000000, -0.000000000000000000, 1.000000000000000000 ) ) ;
#11261 = EDGE_LOOP ( 'NONE', ( #19694, #10079, #8185, #13769 ) ) ;
#11262 = VECTOR ( 'NONE', #3264, 1000.000000000000000 ) ;
#11263 = ORIENTED_EDGE ( 'NONE', *, *, #7031, .T. ) ;
#11264 = ORIENTED_EDGE ( 'NONE', *, *, #20219, .T. ) ;
#11265 = EDGE_CURVE ( 'NONE', #7708, #1300, #9539, .T. ) ;
#11266 = CONTEXT_DEPENDENT_SHAPE_REPRESENTATION ( #826, #12574 ) ;
#11267 = VERTEX_POINT ( 'NONE', #17327 ) ;
#11268 = EDGE_CURVE ( 'NONE', #3720, #17381, #221, .T. ) ;
#11269 = DIRECTION ( 'NONE',  ( 0.8660254037844449249, -0.4999999999999888423, 0.000000000000000000 ) ) ;
#11270 = CARTESIAN_POINT ( 'NONE',  ( -118.0985281540987017, 92.51441522866370804, 44.20207086512186123 ) ) ;
#11271 = ORIENTED_EDGE ( 'NONE', *, *, #17374, .T. ) ;
#11272 = AXIS2_PLACEMENT_3D ( 'NONE', #14426, #8377, #406 ) ;
#11273 = DIRECTION ( 'NONE',  ( 1.000000000000000000, 0.000000000000000000, 0.000000000000000000 ) ) ;
#11274 = LINE ( 'NONE', #6587, #19720 ) ;
#11275 = DIRECTION ( 'NONE',  ( -1.000000000000000000, -0.000000000000000000, -0.000000000000000000 ) ) ;
#11276 = EDGE_CURVE ( 'NONE', #1059, #1114, #6376, .T. ) ;
#11277 = AXIS2_PLACEMENT_3D ( 'NONE', #4910, #7956, #186 ) ;
#11278 = EDGE_CURVE ( 'NONE', #1151, #2847, #15469, .T. ) ;
#11279 = EDGE_CURVE ( 'NONE', #1151, #7965, #6653, .T. ) ;
#11280 = CARTESIAN_POINT ( 'NONE',  ( -129.6868978415389222, 52.87694723226520210, 33.99445347032297349 ) ) ;
#11281 = ADVANCED_FACE ( 'NONE', ( #6175 ), #10855, .T. ) ;
#11282 = DIRECTION ( 'NONE',  ( 6.982962677686266711E-15, -0.000000000000000000, 1.000000000000000000 ) ) ;
#11283 = CARTESIAN_POINT ( 'NONE',  ( -149.5153435750498829, 12.29774247357356565, -1.337809393647938938 ) ) ;
#11284 = DIRECTION ( 'NONE',  ( 0.000000000000000000, 0.000000000000000000, 1.000000000000000000 ) ) ;
#11285 = DIRECTION ( 'NONE',  ( -0.000000000000000000, -0.000000000000000000, 1.000000000000000000 ) ) ;
#11286 = DIRECTION ( 'NONE',  ( 1.000000000000000000, 0.000000000000000000, 0.000000000000000000 ) ) ;
#11287 = ORIENTED_EDGE ( 'NONE', *, *, #8475, .T. ) ;
#11288 = PRODUCT_DEFINITION_SHAPE ( 'NONE', 'NONE',  #1770 ) ;
#11289 = CARTESIAN_POINT ( 'NONE',  ( -139.8142396999972163, 1.712230611238718486E-14, -13.33333333333329307 ) ) ;
#11290 = COLOUR_RGB ( '', 0.09019608, 0.27058824, 0.51372549) ;
#11291 = EDGE_CURVE ( 'NONE', #6744, #13679, #4908, .T. ) ;
#11292 = ORIENTED_EDGE ( 'NONE', *, *, #1732, .F. ) ;
#11293 = ORIENTED_EDGE ( 'NONE', *, *, #15044, .T. ) ;
#11294 = ORIENTED_EDGE ( 'NONE', *, *, #3128, .T. ) ;
#11295 = CARTESIAN_POINT ( 'NONE',  ( 82.03125000000004263, -125.5821405433013780, 10.00000000000000178 ) ) ;
#11296 = AXIS2_PLACEMENT_3D ( 'NONE', #1298, #4360, #10386 ) ;
#11297 = DIRECTION ( 'NONE',  ( 6.982962677686266711E-15, 0.000000000000000000, 1.000000000000000000 ) ) ;
#11298 = DIRECTION ( 'NONE',  ( -0.000000000000000000, -0.000000000000000000, -1.000000000000000000 ) ) ;
#11299 = EDGE_CURVE ( 'NONE', #15754, #13585, #1864, .T. ) ;
#11301 = CARTESIAN_POINT ( 'NONE',  ( 71.18887634719571622, -147.8252249328912740, 49.99999999999999289 ) ) ;
#11300 = VECTOR ( 'NONE', #12136, 1000.000000000000000 ) ;
#11302 = CARTESIAN_POINT ( 'NONE',  ( -136.4621351594848875, -31.11743562882559644, -11.66901485073876010 ) ) ;
#11303 = FACE_OUTER_BOUND ( 'NONE', #3899, .T. ) ;
#11304 = DIRECTION ( 'NONE',  ( -0.7660444431189858960, -0.6427876096865298150, 5.346191897317643224E-15 ) ) ;
#11305 = CARTESIAN_POINT ( 'NONE',  ( 17.50000000000001776, 2.143131898507868643E-15, 49.99999999999999289 ) ) ;
#11306 = DIRECTION ( 'NONE',  ( 1.000000000000000000, 0.000000000000000000, 0.000000000000000000 ) ) ;
#11307 = DIRECTION ( 'NONE',  ( 1.000000000000000000, 0.000000000000000000, 0.000000000000000000 ) ) ;
#11308 = EDGE_CURVE ( 'NONE', #19124, #2439, #9462, .T. ) ;
#11309 = EDGE_LOOP ( 'NONE', ( #2038, #12984 ) ) ;
#11310 = PLANE ( 'NONE',  #16926 ) ;
#11311 = CARTESIAN_POINT ( 'NONE',  ( 132.8189972983174414, -84.37332251142814243, 39.04785267872424726 ) ) ;
#11312 = AXIS2_PLACEMENT_3D ( 'NONE', #7614, #2822, #10574 ) ;
#11313 = ORIENTED_EDGE ( 'NONE', *, *, #17847, .T. ) ;
#11314 = ORIENTED_EDGE ( 'NONE', *, *, #13037, .T. ) ;
#11315 = CLOSED_SHELL ( 'NONE', ( #19654, #3355, #5052, #14738, #12724, #10271, #1216, #4718, #13645, #8744, #5464, #1013, #4133, #18392, #10669, #19616, #12618, #7786, #7641, #10847, #18875, #4466, #2039, #10062, #11003, #11955, #8889, #11486, #1122, #17009, #2869, #3092, #12004, #16784, #16526, #2480, #2114, #12791, #11371, #8147, #2666, #2554, #10468, #603, #4919, #16607, #8827, #18475, #18762, #6620, #841, #10457, #2028, #11226, #16162, #3914, #1842, #15738, #5268, #10344, #6402, #12287, #11879, #14294, #7658, #8975, #3546, #8987, #10878, #11134, #4897, #9407, #849, #3766, #7481, #19842, #8422, #13262, #12513, #11745, #793, #19738, #2229, #4867, #9037, #10459, #2219, #13496, #9120, #1605, #14896, #1016, #8505, #10277, #9384, #7116, #15553, #13719, #18518, #19745, #10644, #9859, #3627, #11585, #14541, #5283, #16358, #18615, #6148, #2655, #16773, #5629, #2990, #19596, #18000, #12810, #16709, #3437, #5732, #20078, #6308, #10840, #1497, #8849, #16847, #6107, #16648, #12612, #400, #14760, #6894, #12634, #8909, #146, #20026, #4518, #523, #1631, #13739, #14741, #9293, #18377, #7760, #16409, #7257, #2412, #7387, #15985, #7874, #15356, #16250, #6111, #1882, #15902, #19351, #16033, #1227, #19066, #10110, #9666, #6677, #13744, #4130, #15119, #469, #13483, #1158, #15353, #17604, #14402, #8286, #7041, #15358, #15145, #14604, #20023, #11899, #2522, #3722, #972, #9992, #1791, #16304, #13589, #3342, #13890, #18782, #14627, #10876, #18306, #16738, #3359, #13387, #10632, #2742, #717, #7474, #4923, #11758, #16554, #7695, #14545, #14672, #2374, #15096, #10636, #2049, #7732, #12913, #5900, #16024, #16046, #7587, #12471, #9486, #10146, #14844, #1635, #14873, #1241, #12538, #16236, #18750, #19195, #15383, #20154, #8107, #5503, #2813, #20155, #1246, #148, #4924, #3040, #17646, #3661, #13953, #20111, #1737, #17865, #9153, #7967, #19242, #1127, #13017, #5886, #7865, #951, #15037, #6564, #2713, #2025, #17022, #19971, #11504, #6473, #17154, #13241, #901, #18208, #18026, #16263, #18747, #2642, #7609, #19042, #16969, #14867, #1404, #3521, #9805, #2733, #16720, #6736, #16401, #1909, #18112, #12921, #10249, #15619, #2117, #20088, #19187, #19154, #6505, #5489, #4858, #13270, #2112, #2795, #10173, #11237, #17775, #124, #7374, #6413, #9775, #17637, #16661, #4547, #17798, #43, #17296, #5039, #2413, #11354 ) ) ;
#11316 = ORIENTED_EDGE ( 'NONE', *, *, #14021, .F. ) ;
#11317 = ORIENTED_EDGE ( 'NONE', *, *, #149, .T. ) ;
#11318 = CARTESIAN_POINT ( 'NONE',  ( 49.67518383744835120, -60.47951622432767493, 132.4711112102474146 ) ) ;
#11319 = AXIS2_PLACEMENT_3D ( 'NONE', #2432, #14899, #5497 ) ;
#11320 = EDGE_LOOP ( 'NONE', ( #12844, #9326, #11497, #17901 ) ) ;
#11321 = CARTESIAN_POINT ( 'NONE',  ( 73.06915264522001507, 28.06281046684300406, 111.4180192758973362 ) ) ;
#11322 = CARTESIAN_POINT ( 'NONE',  ( -103.6579813550139875, -125.0534741538843804, 39.24896055728943622 ) ) ;
#11323 = DIRECTION ( 'NONE',  ( -0.000000000000000000, -0.000000000000000000, 1.000000000000000000 ) ) ;
#11324 = DIRECTION ( 'NONE',  ( -0.1390141521205912334, 0.9902903945359629034, 0.000000000000000000 ) ) ;
#11325 = ORIENTED_EDGE ( 'NONE', *, *, #11246, .T. ) ;
#11326 = CARTESIAN_POINT ( 'NONE',  ( 135.0159133995099410, -65.35183200177810647, 7.107308349490855548 ) ) ;
#11327 = LINE ( 'NONE', #17583, #16630 ) ;
#11328 = AXIS2_PLACEMENT_3D ( 'NONE', #17981, #9994, #13244 ) ;
#11329 = ORIENTED_EDGE ( 'NONE', *, *, #23, .F. ) ;
#11330 = AXIS2_PLACEMENT_3D ( 'NONE', #16293, #5632, #2276 ) ;
#11331 = DIRECTION ( 'NONE',  ( 0.000000000000000000, 0.000000000000000000, 1.000000000000000000 ) ) ;
#11332 = CARTESIAN_POINT ( 'NONE',  ( 0.000000000000000000, 0.000000000000000000, 283.5832628385307999 ) ) ;
#11333 = CARTESIAN_POINT ( 'NONE',  ( 0.000000000000000000, 0.000000000000000000, 283.5832628385307999 ) ) ;
#11334 = EDGE_CURVE ( 'NONE', #18649, #14660, #13696, .T. ) ;
#11335 = DIRECTION ( 'NONE',  ( 0.000000000000000000, 0.000000000000000000, 1.000000000000000000 ) ) ;
#11336 = CIRCLE ( 'NONE', #9696, 7.500000000000007105 ) ;
#11337 = LINE ( 'NONE', #1630, #10348 ) ;
#11338 = CARTESIAN_POINT ( 'NONE',  ( 60.68567895461851691, -2.629250726500488078, 293.5832628385307999 ) ) ;
#11339 = CARTESIAN_POINT ( 'NONE',  ( -77.67451021423168811, 116.4791384160827192, -8.518550530975769419 ) ) ;
#11340 = ORIENTED_EDGE ( 'NONE', *, *, #10979, .T. ) ;
#11341 = DIRECTION ( 'NONE',  ( 1.000000000000000000, 0.000000000000000000, 0.000000000000000000 ) ) ;
#11342 = EDGE_LOOP ( 'NONE', ( #12773, #1764, #2141, #13820 ) ) ;
#11343 = EDGE_LOOP ( 'NONE', ( #14686, #15254, #13919, #19354 ) ) ;
#11344 = DIRECTION ( 'NONE',  ( 1.000000000000000000, 1.613511099790691498E-16, -0.000000000000000000 ) ) ;
#11345 = EDGE_CURVE ( 'NONE', #7430, #12535, #6581, .T. ) ;
#11346 = EDGE_LOOP ( 'NONE', ( #18371, #2082 ) ) ;
#11347 = DIRECTION ( 'NONE',  ( -0.7881095627315599650, -0.6155349844899714595, 0.000000000000000000 ) ) ;
#11348 = CIRCLE ( 'NONE', #13621, 60.74260934110282051 ) ;
#11349 = FACE_BOUND ( 'NONE', #14684, .T. ) ;
#11350 = ORIENTED_EDGE ( 'NONE', *, *, #13614, .T. ) ;
#11351 = CYLINDRICAL_SURFACE ( 'NONE', #15865, 62.91752772691707207 ) ;
#11352 = CARTESIAN_POINT ( 'NONE',  ( 166.7850001792985495, -189.9999999999999432, 40.00000000000000000 ) ) ;
#11353 = CYLINDRICAL_SURFACE ( 'NONE', #19880, 15.91767397667354089 ) ;
#11354 = ADVANCED_FACE ( 'NONE', ( #5150 ), #8600, .T. ) ;
#11355 = DIRECTION ( 'NONE',  ( 1.000000000000000000, 0.000000000000000000, 0.000000000000000000 ) ) ;
#11356 = DIRECTION ( 'NONE',  ( -0.000000000000000000, -0.000000000000000000, 1.000000000000000000 ) ) ;
#11357 = EDGE_CURVE ( 'NONE', #998, #8067, #13000, .T. ) ;
#11358 = CYLINDRICAL_SURFACE ( 'NONE', #19064, 7.500000000000002665 ) ;
#11359 = DIRECTION ( 'NONE',  ( -0.7660444431189865622, -0.6427876096865291489, 5.380491337840971071E-15 ) ) ;
#11360 = CARTESIAN_POINT ( 'NONE',  ( 28.94983032429829350, -53.40245231972188833, 283.5832628385307999 ) ) ;
#11361 = CARTESIAN_POINT ( 'NONE',  ( -140.0000000000000000, 1.714505518806294914E-14, 49.99999999999999289 ) ) ;
#11362 = AXIS2_PLACEMENT_3D ( 'NONE', #1193, #7437, #12549 ) ;
#11363 = ORIENTED_EDGE ( 'NONE', *, *, #9892, .T. ) ;
#11364 = VECTOR ( 'NONE', #2934, 1000.000000000000227 ) ;
#11365 = FACE_OUTER_BOUND ( 'NONE', #2862, .T. ) ;
#11366 = CARTESIAN_POINT ( 'NONE',  ( -49.07263256785925876, 39.37628763770471352, 293.5832628385307999 ) ) ;
#11367 = ORIENTED_EDGE ( 'NONE', *, *, #8758, .T. ) ;
#11368 = ORIENTED_EDGE ( 'NONE', *, *, #16744, .F. ) ;
#11369 = ORIENTED_EDGE ( 'NONE', *, *, #1685, .F. ) ;
#11370 = APPLICATION_PROTOCOL_DEFINITION ( 'draft international standard', 'automotive_design', 1998, #10235 ) ;
#11371 = ADVANCED_FACE ( 'NONE', ( #14643 ), #8300, .T. ) ;
#11372 = EDGE_CURVE ( 'NONE', #15086, #141, #3908, .T. ) ;
#11373 = VERTEX_POINT ( 'NONE', #13187 ) ;
#11374 = EDGE_CURVE ( 'NONE', #4761, #10591, #534, .T. ) ;
#11375 = DIRECTION ( 'NONE',  ( -6.982962677686266711E-15, 0.000000000000000000, -1.000000000000000000 ) ) ;
#11376 = CARTESIAN_POINT ( 'NONE',  ( -148.3536700004592319, 22.27615101400069264, 16.41737317648027883 ) ) ;
#11377 = ORIENTED_EDGE ( 'NONE', *, *, #15761, .T. ) ;
#11378 = DIRECTION ( 'NONE',  ( 0.7660444431189835646, -0.6427876096865328126, 0.000000000000000000 ) ) ;
#11379 = DIRECTION ( 'NONE',  ( 0.3427509529624101492, -0.9394263059140720573, 0.000000000000000000 ) ) ;
#11380 = CARTESIAN_POINT ( 'NONE',  ( -103.0386482854710977, -126.0278359105729891, 1.045141973220539811 ) ) ;
#11381 = CIRCLE ( 'NONE', #19537, 60.74260934110282051 ) ;
#11382 = EDGE_CURVE ( 'NONE', #10980, #11724, #2920, .T. ) ;
#11383 = CARTESIAN_POINT ( 'NONE',  ( -136.5225140300081534, 31.06975746072189892, 27.84628854908055118 ) ) ;
#11384 = EDGE_CURVE ( 'NONE', #11211, #2196, #14446, .T. ) ;
#11385 = CARTESIAN_POINT ( 'NONE',  ( -148.0615764913603698, 24.55031428987399522, -7.575931336099094970 ) ) ;
#11386 = DIRECTION ( 'NONE',  ( 0.4338837391175654479, -0.9009688679024155933, 0.000000000000000000 ) ) ;
#11387 = CARTESIAN_POINT ( 'NONE',  ( 44.89578954330581695, 107.1965464310834477, 14.88498244535514026 ) ) ;
#11388 = ORIENTED_EDGE ( 'NONE', *, *, #18242, .T. ) ;
#11389 = CARTESIAN_POINT ( 'NONE',  ( -122.3581121773129183, 55.09912925957832641, -27.76044880785753577 ) ) ;
#11390 = AXIS2_PLACEMENT_3D ( 'NONE', #16985, #17299, #10935 ) ;
#11391 = CIRCLE ( 'NONE', #8448, 60.74260934110282051 ) ;
#11392 = AXIS2_PLACEMENT_3D ( 'NONE', #9078, #15321, #1200 ) ;
#11393 = AXIS2_PLACEMENT_3D ( 'NONE', #3849, #2328, #8556 ) ;
#11394 = VERTEX_POINT ( 'NONE', #14546 ) ;
#11395 = EDGE_CURVE ( 'NONE', #16596, #2991, #14742, .T. ) ;
#11396 = EDGE_LOOP ( 'NONE', ( #13327, #17160, #471, #16873 ) ) ;
#11397 = EDGE_CURVE ( 'NONE', #1972, #11122, #7071, .T. ) ;
#11398 = VERTEX_POINT ( 'NONE', #432 ) ;
#11399 = CARTESIAN_POINT ( 'NONE',  ( 20.74471755083603952, -59.39925916207552348, 132.4711112102474146 ) ) ;
#11400 = DIRECTION ( 'NONE',  ( 0.000000000000000000, 1.000000000000000000, 0.000000000000000000 ) ) ;
#11401 = CARTESIAN_POINT ( 'NONE',  ( -51.51682027493045979, 28.15057869795642986, 132.4711112102474146 ) ) ;
#11402 = VECTOR ( 'NONE', #7471, 999.9999999999998863 ) ;
#11403 = CARTESIAN_POINT ( 'NONE',  ( -189.9999999999988916, 285.0000000000000568, 12.50000000000027178 ) ) ;
#11404 = VECTOR ( 'NONE', #14277, 1000.000000000000114 ) ;
#11405 = AXIS2_PLACEMENT_3D ( 'NONE', #16832, #16729, #19898 ) ;
#11406 = CARTESIAN_POINT ( 'NONE',  ( -30.74413178637154687, 54.89456854707574252, 132.4711112102474146 ) ) ;
#11407 = AXIS2_PLACEMENT_3D ( 'NONE', #9132, #18240, #4228 ) ;
#11408 = EDGE_CURVE ( 'NONE', #9389, #5911, #3985, .T. ) ;
#11409 = DIRECTION ( 'NONE',  ( -0.5300553768524376430, -0.8479630283625698706, 0.000000000000000000 ) ) ;
#11410 = DIRECTION ( 'NONE',  ( 0.000000000000000000, 0.000000000000000000, 1.000000000000000000 ) ) ;
#11411 = CYLINDRICAL_SURFACE ( 'NONE', #14072, 32.50000000000000000 ) ;
#11412 = DIRECTION ( 'NONE',  ( -1.000000000000000000, 0.000000000000000000, 0.000000000000000000 ) ) ;
#11413 = VERTEX_POINT ( 'NONE', #8696 ) ;
#11414 = DIRECTION ( 'NONE',  ( -0.000000000000000000, -0.000000000000000000, 1.000000000000000000 ) ) ;
#11415 = ORIENTED_EDGE ( 'NONE', *, *, #10953, .F. ) ;
#11416 = ORIENTED_EDGE ( 'NONE', *, *, #1658, .F. ) ;
#11417 = ORIENTED_EDGE ( 'NONE', *, *, #2895, .F. ) ;
#11418 = EDGE_CURVE ( 'NONE', #15200, #14483, #19641, .T. ) ;
#11419 = EDGE_CURVE ( 'NONE', #2611, #6324, #12054, .T. ) ;
#11420 = AXIS2_PLACEMENT_3D ( 'NONE', #15779, #4842, #14036 ) ;
#11421 = CIRCLE ( 'NONE', #13697, 60.74260934110282051 ) ;
#11422 = ORIENTED_EDGE ( 'NONE', *, *, #19231, .T. ) ;
#11423 = ORIENTED_EDGE ( 'NONE', *, *, #18462, .F. ) ;
#11424 = DIRECTION ( 'NONE',  ( 0.000000000000000000, 0.000000000000000000, 1.000000000000000000 ) ) ;
#11425 = EDGE_CURVE ( 'NONE', #195, #18230, #2465, .T. ) ;
#11426 = DIRECTION ( 'NONE',  ( 0.1736481776669207000, 0.9848077530122097967, 0.000000000000000000 ) ) ;
#11427 = DIRECTION ( 'NONE',  ( 0.1736481776669241417, 0.9848077530122091305, 0.000000000000000000 ) ) ;
#11428 = DIRECTION ( 'NONE',  ( -1.000000000000000000, 0.000000000000000000, 0.000000000000000000 ) ) ;
#11429 = EDGE_LOOP ( 'NONE', ( #18835, #15386, #19864, #19205 ) ) ;
#11430 = CARTESIAN_POINT ( 'NONE',  ( 134.3888575020695555, -66.63121209263867684, 2.991575443300840575 ) ) ;
#11431 = DIRECTION ( 'NONE',  ( 1.000000000000000000, 0.000000000000000000, 0.000000000000000000 ) ) ;
#11432 = EDGE_LOOP ( 'NONE', ( #1593, #19546, #9942, #20012 ) ) ;
#11433 = DIRECTION ( 'NONE',  ( 0.000000000000000000, 1.000000000000000000, 0.000000000000000000 ) ) ;
#11434 = DIRECTION ( 'NONE',  ( 1.000000000000000000, 0.000000000000000000, 0.000000000000000000 ) ) ;
#11435 = DIRECTION ( 'NONE',  ( -0.7660444431189862291, -0.6427876096865298150, 4.304393070272780959E-15 ) ) ;
#11436 = DIRECTION ( 'NONE',  ( -0.7660444431189707970, -0.6427876096865481337, 0.000000000000000000 ) ) ;
#11437 = LINE ( 'NONE', #3756, #8412 ) ;
#11438 = DIRECTION ( 'NONE',  ( -0.5300553768524376430, -0.8479630283625698706, 0.000000000000000000 ) ) ;
#11439 = CARTESIAN_POINT ( 'NONE',  ( 82.89467276472738888, -125.0139572091429869, 36.00987770447442671 ) ) ;
#11440 = ORIENTED_EDGE ( 'NONE', *, *, #9095, .F. ) ;
#11441 = CARTESIAN_POINT ( 'NONE',  ( -78.26059000578311498, 0.8220851292432594937, 132.4711112102474146 ) ) ;
#11442 = VERTEX_POINT ( 'NONE', #15134 ) ;
#11443 = ORIENTED_EDGE ( 'NONE', *, *, #6675, .T. ) ;
#11444 = CARTESIAN_POINT ( 'NONE',  ( 0.000000000000000000, 0.000000000000000000, 293.5832628385307999 ) ) ;
#11445 = EDGE_LOOP ( 'NONE', ( #14976, #6595, #9638, #16564 ) ) ;
#11446 = VECTOR ( 'NONE', #4431, 1000.000000000000114 ) ;
#11447 = DIRECTION ( 'NONE',  ( -0.000000000000000000, -0.000000000000000000, -1.000000000000000000 ) ) ;
#11448 = FACE_OUTER_BOUND ( 'NONE', #8596, .T. ) ;
#11449 = CARTESIAN_POINT ( 'NONE',  ( 0.000000000000000000, 0.000000000000000000, 49.99999999999999289 ) ) ;
#11450 = CARTESIAN_POINT ( 'NONE',  ( 0.000000000000000000, 0.000000000000000000, 39.99999999999999289 ) ) ;
#11451 = LINE ( 'NONE', #4530, #9519 ) ;
#11452 = PRODUCT_DEFINITION_SHAPE ( 'NONE', 'NONE',  #20252 ) ;
#11453 = LINE ( 'NONE', #16271, #4796 ) ;
#11454 = CARTESIAN_POINT ( 'NONE',  ( 100.4560359297608585, -129.9019447003570349, 2.893739865237928033 ) ) ;
#11455 = DIRECTION ( 'NONE',  ( -0.000000000000000000, -0.000000000000000000, -1.000000000000000000 ) ) ;
#11456 = DIRECTION ( 'NONE',  ( 0.9396926207859063185, -0.3420201433256742640, -6.456589605409180904E-15 ) ) ;
#11457 = DIRECTION ( 'NONE',  ( -0.000000000000000000, -0.000000000000000000, 1.000000000000000000 ) ) ;
#11458 = DIRECTION ( 'NONE',  ( 1.000000000000000000, 0.000000000000000000, 0.000000000000000000 ) ) ;
#11459 = CARTESIAN_POINT ( 'NONE',  ( 91.69207598197974107, -118.7138234487252078, -7.504338834299504768 ) ) ;
#11460 = CIRCLE ( 'NONE', #1324, 7.500000000000001776 ) ;
#11461 = CARTESIAN_POINT ( 'NONE',  ( -109.5721339228235820, 31.03941509555038181, 39.88498244535622206 ) ) ;
#11462 = ORIENTED_EDGE ( 'NONE', *, *, #12123, .F. ) ;
#11463 = DIRECTION ( 'NONE',  ( 1.000000000000000000, 3.129754055707530415E-16, -0.000000000000000000 ) ) ;
#11464 = CARTESIAN_POINT ( 'NONE',  ( -110.0000000000000284, 101.9803902718557111, 44.99999999999998579 ) ) ;
#11465 = ORIENTED_EDGE ( 'NONE', *, *, #20028, .F. ) ;
#11466 = ORIENTED_EDGE ( 'NONE', *, *, #14377, .F. ) ;
#11467 = ORIENTED_EDGE ( 'NONE', *, *, #3272, .F. ) ;
#11468 = ORIENTED_EDGE ( 'NONE', *, *, #16774, .T. ) ;
#11469 = EDGE_CURVE ( 'NONE', #4599, #11965, #5944, .T. ) ;
#11470 = AXIS2_PLACEMENT_3D ( 'NONE', #11716, #3951, #7131 ) ;
#11471 = DIRECTION ( 'NONE',  ( -1.000000000000000000, 0.000000000000000000, 0.000000000000000000 ) ) ;
#11472 = ORIENTED_EDGE ( 'NONE', *, *, #8007, .F. ) ;
#11473 = CIRCLE ( 'NONE', #13751, 12.50000000000006750 ) ;
#11474 = DIRECTION ( 'NONE',  ( 0.000000000000000000, -0.000000000000000000, 1.000000000000000000 ) ) ;
#11475 = CARTESIAN_POINT ( 'NONE',  ( -96.93610878393819519, -115.7104363121878094, 10.35199856087829673 ) ) ;
#11476 = VERTEX_POINT ( 'NONE', #19941 ) ;
#11477 = EDGE_CURVE ( 'NONE', #6802, #13175, #13044, .T. ) ;
#11478 = CARTESIAN_POINT ( 'NONE',  ( 114.2960429025578293, -28.68569479505797659, 39.88498244535465176 ) ) ;
#11479 = EDGE_CURVE ( 'NONE', #1034, #14947, #11757, .T. ) ;
#11480 = CARTESIAN_POINT ( 'NONE',  ( 18.28503710798548454, -57.92514141135459482, 293.5832628385307999 ) ) ;
#11481 = ADVANCED_FACE ( 'NONE', ( #2768 ), #19737, .T. ) ;
#11482 = SHAPE_REPRESENTATION_RELATIONSHIP ( 'NONE' , 'NONE' ,  #5472, #15283 ) ;
#11483 = FACE_BOUND ( 'NONE', #15137, .T. ) ;
#11484 = FACE_OUTER_BOUND ( 'NONE', #7879, .T. ) ;
#11485 = VERTEX_POINT ( 'NONE', #7176 ) ;
#11486 = ADVANCED_FACE ( 'NONE', ( #11849 ), #12158, .T. ) ;
#11487 = DIRECTION ( 'NONE',  ( 1.000000000000000000, -0.000000000000000000, -0.000000000000000000 ) ) ;
#11488 = ORIENTED_EDGE ( 'NONE', *, *, #11419, .F. ) ;
#11489 = ORIENTED_EDGE ( 'NONE', *, *, #12737, .T. ) ;
#11490 = EDGE_CURVE ( 'NONE', #14482, #8290, #19907, .T. ) ;
#11491 = ORIENTED_EDGE ( 'NONE', *, *, #12661, .F. ) ;
#11492 = DIRECTION ( 'NONE',  ( 0.2225209339563044841, 0.9749279121818258398, 0.000000000000000000 ) ) ;
#11493 = B_SPLINE_CURVE_WITH_KNOTS ( 'NONE', 3,
 ( #11900, #12003, #9149, #18261, #12102, #5992, #2512, #15390, #18362, #4340, #12211, #10675, #16930, #18781, #251, #8021, #11189, #4762, #4553, #9356, #17454, #152, #8122, #3326, #4658, #17140, #11086, #51, #12621, #14268, #15707, #12309, #1583, #18882, #13952, #14063, #10984, #9564, #6503, #15496, #1483, #18987 ),
 .UNSPECIFIED., .F., .F.,
 ( 4, 2, 2, 2, 2, 2, 2, 2, 2, 2, 2, 2, 2, 2, 2, 2, 2, 2, 2, 2, 4 ),
 ( -0.03221374292090079666, -0.02616091102393758305, -0.02464770304969675710, -0.02313449507545593115, -0.02010807912697429312, -0.01708166317849265509, -0.01556845520425183260, -0.01405524723001101359, -0.01102883128152938250, -0.009515623307288563482, -0.008002415333047747936, -0.004975999384566141132, -0.001949583436084537796, 0.001076832512397069008, 0.004103248460878679282, 0.007129664409360289556, 0.008642872383601091224, 0.01015608035784189289, 0.01318249630632349623, 0.01469570428056430483, 0.01620891225480510650 ),
 .UNSPECIFIED. ) ;
#11494 = CARTESIAN_POINT ( 'NONE',  ( -131.6317334595287605, -71.92650142027846982, -4.251463035882792063 ) ) ;
#11495 = DIRECTION ( 'NONE',  ( -0.7660444431189865622, -0.6427876096865291489, 4.304393070272777014E-15 ) ) ;
#11496 = CARTESIAN_POINT ( 'NONE',  ( 0.3593302862868668068, 3.504574740656555498, -9.000000000000000000 ) ) ;
#11497 = ORIENTED_EDGE ( 'NONE', *, *, #16188, .T. ) ;
#11498 = LINE ( 'NONE', #2205, #5858 ) ;
#11499 = CARTESIAN_POINT ( 'NONE',  ( -123.3142212418527350, -85.40728428758222890, -0.3493686248430047381 ) ) ;
#11500 = EDGE_CURVE ( 'NONE', #6137, #2972, #18317, .T. ) ;
#11501 = CARTESIAN_POINT ( 'NONE',  ( -1.379293853801755176, 58.69016442926522359, 112.7772637782949943 ) ) ;
#11502 = FACE_OUTER_BOUND ( 'NONE', #7196, .T. ) ;
#11503 = AXIS2_PLACEMENT_3D ( 'NONE', #19191, #10992, #17562 ) ;
#11504 = ADVANCED_FACE ( 'NONE', ( #15232 ), #1221, .F. ) ;
#11505 = CARTESIAN_POINT ( 'NONE',  ( 102.1629267457074519, -127.3823967956316210, 38.47850501251131305 ) ) ;
#11506 = CARTESIAN_POINT ( 'NONE',  ( -31.77187437101504486, -51.77076963420836364, 283.5832628385307999 ) ) ;
#11507 = EDGE_CURVE ( 'NONE', #18211, #9562, #10072, .T. ) ;
#11508 = VERTEX_POINT ( 'NONE', #2562 ) ;
#11509 = ORIENTED_EDGE ( 'NONE', *, *, #13991, .F. ) ;
#11510 = ORIENTED_EDGE ( 'NONE', *, *, #247, .F. ) ;
#11511 = VERTEX_POINT ( 'NONE', #16485 ) ;
#11512 = ORIENTED_EDGE ( 'NONE', *, *, #7489, .T. ) ;
#11513 = CARTESIAN_POINT ( 'NONE',  ( -166.7850001792984926, -200.0000000000000284, 40.00000000000000000 ) ) ;
#11514 = EDGE_CURVE ( 'NONE', #912, #2184, #18113, .T. ) ;
#11515 = CIRCLE ( 'NONE', #18051, 7.500000000000001776 ) ;
#11516 = AXIS2_PLACEMENT_3D ( 'NONE', #10944, #12475, #414 ) ;
#11517 = ORIENTED_EDGE ( 'NONE', *, *, #762, .T. ) ;
#11518 = DIRECTION ( 'NONE',  ( 0.000000000000000000, 0.000000000000000000, 1.000000000000000000 ) ) ;
#11519 = DIRECTION ( 'NONE',  ( 0.000000000000000000, 0.000000000000000000, 1.000000000000000000 ) ) ;
#11520 = PLANE ( 'NONE',  #12321 ) ;
#11521 = ORIENTED_EDGE ( 'NONE', *, *, #10862, .F. ) ;
#11522 = VECTOR ( 'NONE', #18329, 1000.000000000000000 ) ;
#11523 = CARTESIAN_POINT ( 'NONE',  ( 0.000000000000000000, 0.000000000000000000, -115.0000000000000142 ) ) ;
#11524 = CARTESIAN_POINT ( 'NONE',  ( -97.49999999999998579, -113.9901311517800337, 10.00000000000000178 ) ) ;
#11525 = EDGE_LOOP ( 'NONE', ( #3340, #10696 ) ) ;
#11526 = FACE_OUTER_BOUND ( 'NONE', #17294, .T. ) ;
#11527 = DIRECTION ( 'NONE',  ( 6.982962677686266711E-15, -0.000000000000000000, 1.000000000000000000 ) ) ;
#11528 = EDGE_CURVE ( 'NONE', #15281, #16710, #10322, .T. ) ;
#11529 = DIRECTION ( 'NONE',  ( -1.000000000000000000, 0.000000000000000000, 0.000000000000000000 ) ) ;
#11530 = ADVANCED_FACE ( 'NONE', ( #7263 ), #13487, .T. ) ;
#11531 = AXIS2_PLACEMENT_3D ( 'NONE', #2262, #19532, #17614 ) ;
#11532 = CARTESIAN_POINT ( 'NONE',  ( -137.8571306610627971, -24.85219049267718106, -16.19534811600425428 ) ) ;
#11533 = DIRECTION ( 'NONE',  ( -6.982962677686266711E-15, 0.000000000000000000, -1.000000000000000000 ) ) ;
#11534 = LINE ( 'NONE', #19511, #11949 ) ;
#11535 = EDGE_CURVE ( 'NONE', #3199, #1414, #18939, .T. ) ;
#11536 = VERTEX_POINT ( 'NONE', #3374 ) ;
#11537 = DIRECTION ( 'NONE',  ( -1.000000000000000000, 0.000000000000000000, 0.000000000000000000 ) ) ;
#11538 = EDGE_CURVE ( 'NONE', #7342, #10874, #2565, .T. ) ;
#11539 = VERTEX_POINT ( 'NONE', #6046 ) ;
#11540 = VECTOR ( 'NONE', #11210, 1000.000000000000114 ) ;
#11541 = EDGE_LOOP ( 'NONE', ( #8445, #4997, #19607 ) ) ;
#11542 = PLANE ( 'NONE',  #14158 ) ;
#11543 = CIRCLE ( 'NONE', #14811, 110.0000000000000142 ) ;
#11544 = ORIENTED_EDGE ( 'NONE', *, *, #13641, .F. ) ;
#11545 = DIRECTION ( 'NONE',  ( -0.9902903945359624593, -0.1390141521205945918, 0.000000000000000000 ) ) ;
#11546 = CARTESIAN_POINT ( 'NONE',  ( -93.79892245610578527, -117.0565612855932329, 48.57152639572796460 ) ) ;
#11547 = CIRCLE ( 'NONE', #12842, 7.500000000000007105 ) ;
#11548 = DIRECTION ( 'NONE',  ( -0.000000000000000000, -0.000000000000000000, 1.000000000000000000 ) ) ;
#11549 = DIRECTION ( 'NONE',  ( 1.000000000000000000, 0.000000000000000000, 0.000000000000000000 ) ) ;
#11550 = ORIENTED_EDGE ( 'NONE', *, *, #5881, .T. ) ;
#11551 = DIRECTION ( 'NONE',  ( -0.000000000000000000, -0.000000000000000000, -1.000000000000000000 ) ) ;
#11552 = DIRECTION ( 'NONE',  ( 1.047444401652940164E-14, -1.000000000000000000, 0.000000000000000000 ) ) ;
#11553 = AXIS2_PLACEMENT_3D ( 'NONE', #5267, #17744, #5363 ) ;
#11554 = CARTESIAN_POINT ( 'NONE',  ( 76.92888220842485225, -14.39940464655733976, 132.4711112102474146 ) ) ;
#11555 = LINE ( 'NONE', #7057, #10584 ) ;
#11556 = ORIENTED_EDGE ( 'NONE', *, *, #12097, .T. ) ;
#11557 = PLANE ( 'NONE',  #13135 ) ;
#11558 = CARTESIAN_POINT ( 'NONE',  ( -73.82206860051547892, -25.99419088092166774, 248.9926560891072143 ) ) ;
#11559 = CARTESIAN_POINT ( 'NONE',  ( 93.26156191356916736, -117.4850166029420535, -8.331654811393381266 ) ) ;
#11560 = LINE ( 'NONE', #11257, #5327 ) ;
#11561 = EDGE_CURVE ( 'NONE', #19232, #9791, #9129, .T. ) ;
#11562 = EDGE_LOOP ( 'NONE', ( #13091, #19261, #17573, #11942 ) ) ;
#11563 = DIRECTION ( 'NONE',  ( 0.000000000000000000, 0.000000000000000000, 1.000000000000000000 ) ) ;
#11564 = CARTESIAN_POINT ( 'NONE',  ( 1.396592535537253342E-14, 0.000000000000000000, 60.00000000000000000 ) ) ;
#11565 = ORIENTED_EDGE ( 'NONE', *, *, #7018, .T. ) ;
#11566 = ORIENTED_EDGE ( 'NONE', *, *, #18004, .F. ) ;
#11567 = VERTEX_POINT ( 'NONE', #17399 ) ;
#11568 = AXIS2_PLACEMENT_3D ( 'NONE', #16295, #8205, #5345 ) ;
#11569 = ORIENTED_EDGE ( 'NONE', *, *, #11397, .F. ) ;
#11570 = DIRECTION ( 'NONE',  ( 0.000000000000000000, 0.000000000000000000, -1.000000000000000000 ) ) ;
#11571 = DIRECTION ( 'NONE',  ( -0.8660254037844344888, -0.5000000000000069944, 0.000000000000000000 ) ) ;
#11572 = AXIS2_PLACEMENT_3D ( 'NONE', #9661, #7712, #18988 ) ;
#11573 = VERTEX_POINT ( 'NONE', #9410 ) ;
#11574 = CARTESIAN_POINT ( 'NONE',  ( -7.948651060879021735, 60.22029172860445101, 293.5832628385307999 ) ) ;
#11575 = CARTESIAN_POINT ( 'NONE',  ( -3.428789370485404223E-15, 8.014718854569430562, 4.118099735505520442 ) ) ;
#11576 = CARTESIAN_POINT ( 'NONE',  ( -96.67218534448896605, -115.8154871359607796, 10.27722555384923098 ) ) ;
#11577 = EDGE_LOOP ( 'NONE', ( #13825, #11363, #18805 ) ) ;
#11578 = LINE ( 'NONE', #19460, #4253 ) ;
#11579 = CARTESIAN_POINT ( 'NONE',  ( -77.21438937758510690, -12.78021302872823384, 132.4711112102474146 ) ) ;
#11580 = FACE_BOUND ( 'NONE', #9728, .T. ) ;
#11581 = VECTOR ( 'NONE', #12377, 1000.000000000000000 ) ;
#11582 = LINE ( 'NONE', #13200, #978 ) ;
#11583 = CARTESIAN_POINT ( 'NONE',  ( 0.000000000000000000, 0.000000000000000000, -10.00000000000000178 ) ) ;
#11584 = DIRECTION ( 'NONE',  ( -0.000000000000000000, -1.000000000000000000, -0.000000000000000000 ) ) ;
#11585 = ADVANCED_FACE ( 'NONE', ( #99 ), #1731, .T. ) ;
#11586 = ORIENTED_EDGE ( 'NONE', *, *, #16412, .T. ) ;
#11587 = DIRECTION ( 'NONE',  ( -0.9993852124581887875, 0.03505990758545545621, 0.000000000000000000 ) ) ;
#11588 = AXIS2_PLACEMENT_3D ( 'NONE', #20052, #1120, #924 ) ;
#11589 = ORIENTED_EDGE ( 'NONE', *, *, #15239, .F. ) ;
#11590 = EDGE_CURVE ( 'NONE', #7769, #13278, #14371, .T. ) ;
#11591 = ORIENTED_EDGE ( 'NONE', *, *, #18680, .F. ) ;
#11592 = VECTOR ( 'NONE', #15117, 1000.000000000000114 ) ;
#11593 = DIRECTION ( 'NONE',  ( 0.000000000000000000, 0.000000000000000000, 1.000000000000000000 ) ) ;
#11594 = DIRECTION ( 'NONE',  ( 0.000000000000000000, 0.000000000000000000, -1.000000000000000000 ) ) ;
#11595 = LINE ( 'NONE', #658, #7448 ) ;
#11596 = DIRECTION ( 'NONE',  ( 0.1736481776669404620, -0.9848077530122062440, 0.000000000000000000 ) ) ;
#11597 = CARTESIAN_POINT ( 'NONE',  ( -87.49999999999998579, -133.9542832461881687, 49.99999999999999289 ) ) ;
#11598 = CARTESIAN_POINT ( 'NONE',  ( -129.7881937802468428, -75.28665481071030285, 0.5105156109461032043 ) ) ;
#11599 = DIRECTION ( 'NONE',  ( 0.9396926207859105373, 0.3420201433256631063, -6.577611345862942596E-15 ) ) ;
#11600 = CARTESIAN_POINT ( 'NONE',  ( 0.000000000000000000, 0.000000000000000000, 49.99999999999999289 ) ) ;
#11601 = CIRCLE ( 'NONE', #13225, 62.91752772691707207 ) ;
#11602 = CARTESIAN_POINT ( 'NONE',  ( 38.41834839689379777, -68.18670162478818497, 110.9660488491356887 ) ) ;
#11603 = EDGE_CURVE ( 'NONE', #13285, #5634, #11736, .T. ) ;
#11604 = ORIENTED_EDGE ( 'NONE', *, *, #4334, .T. ) ;
#11605 = ORIENTED_EDGE ( 'NONE', *, *, #12964, .F. ) ;
#11606 = ORIENTED_EDGE ( 'NONE', *, *, #9559, .T. ) ;
#11607 = CIRCLE ( 'NONE', #10621, 160.0000000000000284 ) ;
#11608 = ORIENTED_EDGE ( 'NONE', *, *, #6909, .T. ) ;
#11609 = CARTESIAN_POINT ( 'NONE',  ( 8.939227532413712041, -60.08331549348429235, 293.5832628385307999 ) ) ;
#11610 = EDGE_CURVE ( 'NONE', #599, #3934, #18516, .T. ) ;
#11611 = ORIENTED_EDGE ( 'NONE', *, *, #6486, .T. ) ;
#11612 = VECTOR ( 'NONE', #4171, 1000.000000000000000 ) ;
#11613 = EDGE_CURVE ( 'NONE', #65, #11160, #10396, .T. ) ;
#11614 = LINE ( 'NONE', #8346, #16450 ) ;
#11615 = FACE_OUTER_BOUND ( 'NONE', #14100, .T. ) ;
#11616 = PLANE ( 'NONE',  #9417 ) ;
#11617 = ORIENTED_EDGE ( 'NONE', *, *, #13698, .F. ) ;
#11618 = CARTESIAN_POINT ( 'NONE',  ( 0.000000000000000000, 0.000000000000000000, 293.5832628385307999 ) ) ;
#11619 = CARTESIAN_POINT ( 'NONE',  ( 18.28503710798548099, -57.92514141135459482, 283.5832628385307999 ) ) ;
#11620 = VERTEX_POINT ( 'NONE', #13801 ) ;
#11621 = DIRECTION ( 'NONE',  ( -0.7660444431189771253, -0.6427876096865404731, 0.000000000000000000 ) ) ;
#11622 = CARTESIAN_POINT ( 'NONE',  ( 58.83691981461632992, -22.28973221005101024, 293.5832628385307999 ) ) ;
#11623 = DIRECTION ( 'NONE',  ( 0.000000000000000000, 0.000000000000000000, -1.000000000000000000 ) ) ;
#11624 = CARTESIAN_POINT ( 'NONE',  ( 0.000000000000000000, 0.000000000000000000, 248.9926560891072143 ) ) ;
#11625 = AXIS2_PLACEMENT_3D ( 'NONE', #11618, #872, #16538 ) ;
#11626 = EDGE_CURVE ( 'NONE', #16701, #19189, #9751, .T. ) ;
#11627 = DIRECTION ( 'NONE',  ( 0.9396926207859058744, -0.3420201433256756518, -6.577611345862941807E-15 ) ) ;
#11628 = CARTESIAN_POINT ( 'NONE',  ( 76.83212392882491315, 14.94814811854986658, 112.0427633081291816 ) ) ;
#11629 = FACE_OUTER_BOUND ( 'NONE', #15920, .T. ) ;
#11630 = EDGE_LOOP ( 'NONE', ( #17645, #5342, #17311, #5682 ) ) ;
#11631 = CARTESIAN_POINT ( 'NONE',  ( 138.2024300533213932, 89.85329105948596862, 39.99999999999999289 ) ) ;
#11632 = VERTEX_POINT ( 'NONE', #15444 ) ;
#11633 = ORIENTED_EDGE ( 'NONE', *, *, #15285, .T. ) ;
#11634 = CARTESIAN_POINT ( 'NONE',  ( -159.9599531637108782, -36.50981547337168109, 49.99999999999999289 ) ) ;
#11635 = ORIENTED_EDGE ( 'NONE', *, *, #1789, .T. ) ;
#11636 = EDGE_CURVE ( 'NONE', #15281, #18849, #1434, .T. ) ;
#11637 = VECTOR ( 'NONE', #2230, 1000.000000000000000 ) ;
#11638 = EDGE_CURVE ( 'NONE', #9538, #14807, #6147, .T. ) ;
#11639 = LINE ( 'NONE', #303, #15964 ) ;
#11640 = CLOSED_SHELL ( 'NONE', ( #3237, #105, #10273, #15293, #17789, #3046, #17131, #16303, #17007, #4747, #2834, #12112, #12404, #7668, #11044, #19629, #18219, #3482, #6511, #4653, #17887, #17667, #6683, #16501, #8093, #19416, #7795, #3423, #14024, #7335, #6870, #15790, #16053, #13707, #5506, #5981, #7132, #7284, #18145, #10570, #851, #3802, #9829, #10762, #8494, #11019, #11530, #14101, #7628, #16922, #8345, #19787, #6052, #7264, #16990, #9639, #9475, #15091, #14721, #14174, #12138, #18564, #19284, #15995, #5717, #2987 ) ) ;
#11641 = CARTESIAN_POINT ( 'NONE',  ( -87.79934266039366264, -121.6207432329495788, 44.44620747261014770 ) ) ;
#11642 = CARTESIAN_POINT ( 'NONE',  ( 87.10655032386927132, -147.8252249328912740, 49.99999999999999289 ) ) ;
#11643 = CARTESIAN_POINT ( 'NONE',  ( -135.1060089022256818, -65.16414933467417825, 49.99999999999999289 ) ) ;
#11644 = ORIENTED_EDGE ( 'NONE', *, *, #13878, .F. ) ;
#11645 = VECTOR ( 'NONE', #11414, 1000.000000000000000 ) ;
#11646 = DIRECTION ( 'NONE',  ( 0.3420201433256663259, 0.9396926207859093161, 0.000000000000000000 ) ) ;
#11647 = CARTESIAN_POINT ( 'NONE',  ( 97.63639055817486678, -133.7757280588254218, 8.337148639838481756 ) ) ;
#11648 = FACE_OUTER_BOUND ( 'NONE', #16191, .T. ) ;
#11649 = DIRECTION ( 'NONE',  ( -0.4338837391175651703, 0.9009688679024158153, -0.000000000000000000 ) ) ;
#11650 = PLANE ( 'NONE',  #5651 ) ;
#11651 = ADVANCED_FACE ( 'NONE', ( #14421 ), #5314, .T. ) ;
#11652 = DIRECTION ( 'NONE',  ( 6.982962677686266711E-15, -0.000000000000000000, 1.000000000000000000 ) ) ;
#11653 = CARTESIAN_POINT ( 'NONE',  ( 82.39904996721719499, -125.3411509769705674, 6.041691364002039322 ) ) ;
#11654 = CARTESIAN_POINT ( 'NONE',  ( 58.69016442926523069, -0.8220851292429179891, 112.7772637782949516 ) ) ;
#11655 = AXIS2_PLACEMENT_3D ( 'NONE', #2929, #2722, #4562 ) ;
#11656 = ORIENTED_EDGE ( 'NONE', *, *, #11418, .F. ) ;
#11657 = DIRECTION ( 'NONE',  ( 1.000000000000000000, 0.000000000000000000, 0.000000000000000000 ) ) ;
#11658 = FACE_OUTER_BOUND ( 'NONE', #4177, .T. ) ;
#11659 = VERTEX_POINT ( 'NONE', #6750 ) ;
#11660 = ORIENTED_EDGE ( 'NONE', *, *, #10003, .T. ) ;
#11661 = AXIS2_PLACEMENT_3D ( 'NONE', #14826, #11652, #2163 ) ;
#11662 = AXIS2_PLACEMENT_3D ( 'NONE', #7300, #4232, #16715 ) ;
#11663 = EDGE_CURVE ( 'NONE', #11539, #9195, #9810, .T. ) ;
#11664 = CARTESIAN_POINT ( 'NONE',  ( 4.189777606611760026E-13, -60.00000000000000000, -105.0000000000000142 ) ) ;
#11665 = CARTESIAN_POINT ( 'NONE',  ( -21.36933070621726571, 54.67896814532662830, 111.4180192758973931 ) ) ;
#11666 = VERTEX_POINT ( 'NONE', #5219 ) ;
#11667 = CARTESIAN_POINT ( 'NONE',  ( 102.7594822686537128, -126.4624059756590526, 1.189579947717209096 ) ) ;
#11668 = CARTESIAN_POINT ( 'NONE',  ( -90.39157087501804710, -119.7120742831093452, -6.695055702633337269 ) ) ;
#11669 = ORIENTED_EDGE ( 'NONE', *, *, #17691, .T. ) ;
#11670 = EDGE_CURVE ( 'NONE', #19563, #10038, #14617, .T. ) ;
#11671 = AXIS2_PLACEMENT_3D ( 'NONE', #3349, #5098, #9388 ) ;
#11672 = CARTESIAN_POINT ( 'NONE',  ( -82.89467276472737467, -125.0139572091430722, 3.990122295525602603 ) ) ;
#11673 = CARTESIAN_POINT ( 'NONE',  ( -32.30548103355219780, 113.3261241031799926, 39.88498244535568205 ) ) ;
#11674 = AXIS2_PLACEMENT_3D ( 'NONE', #5593, #9901, #19605 ) ;
#11675 = CARTESIAN_POINT ( 'NONE',  ( -50.37374754117255549, -141.2886604036510221, 49.99999999999999289 ) ) ;
#11676 = VECTOR ( 'NONE', #1801, 1000.000000000000000 ) ;
#11677 = LINE ( 'NONE', #4001, #19568 ) ;
#11678 = CARTESIAN_POINT ( 'NONE',  ( -189.9999999999988916, 275.0000000000000000, 5.000000000000268230 ) ) ;
#11679 = ORIENTED_EDGE ( 'NONE', *, *, #18359, .T. ) ;
#11680 = DIRECTION ( 'NONE',  ( 0.000000000000000000, 0.000000000000000000, -1.000000000000000000 ) ) ;
#11681 = CARTESIAN_POINT ( 'NONE',  ( 60.72279549541555355, -1.629937663769388090, 283.5832628385307999 ) ) ;
#11682 = EDGE_LOOP ( 'NONE', ( #2838, #3148, #15441 ) ) ;
#11683 = ORIENTED_EDGE ( 'NONE', *, *, #9380, .F. ) ;
#11684 = VECTOR ( 'NONE', #362, 1000.000000000000000 ) ;
#11685 = ORIENTED_EDGE ( 'NONE', *, *, #8735, .T. ) ;
#11686 = CARTESIAN_POINT ( 'NONE',  ( -140.0000000000000284, 1.714505518806294914E-14, -115.0000000000000142 ) ) ;
#11687 = DIRECTION ( 'NONE',  ( 1.000000000000000000, 0.000000000000000000, -0.000000000000000000 ) ) ;
#11688 = CARTESIAN_POINT ( 'NONE',  ( 45.46865632508072963, -40.28046525994365368, 293.5832628385307999 ) ) ;
#11689 = DIRECTION ( 'NONE',  ( -3.491481338843133355E-15, 1.000000000000000000, 0.000000000000000000 ) ) ;
#11690 = ORIENTED_EDGE ( 'NONE', *, *, #2497, .T. ) ;
#11691 = DIRECTION ( 'NONE',  ( -0.6427876096865481337, 0.7660444431189707970, 0.000000000000000000 ) ) ;
#11692 = CARTESIAN_POINT ( 'NONE',  ( -133.0662791979961810, -83.15705346519905561, 1.302451894195027160 ) ) ;
#11693 = DIRECTION ( 'NONE',  ( -0.3427509529624095941, -0.9394263059140722794, 0.000000000000000000 ) ) ;
#11694 = DIRECTION ( 'NONE',  ( 1.000000000000000000, 0.000000000000000000, 0.000000000000000000 ) ) ;
#11695 = DIRECTION ( 'NONE',  ( -0.5000000000000069944, 0.8660254037844345998, 0.000000000000000000 ) ) ;
#11696 = VECTOR ( 'NONE', #2561, 1000.000000000000000 ) ;
#11697 = VERTEX_POINT ( 'NONE', #6846 ) ;
#11698 = CONICAL_SURFACE ( 'NONE', #20193, 9.000000000000000000, 1.047197551196600296 ) ;
#11699 = ORIENTED_EDGE ( 'NONE', *, *, #4359, .T. ) ;
#11700 = ORIENTED_EDGE ( 'NONE', *, *, #13848, .F. ) ;
#11701 = ORIENTED_EDGE ( 'NONE', *, *, #258, .F. ) ;
#11702 = ORIENTED_EDGE ( 'NONE', *, *, #17799, .T. ) ;
#11703 = AXIS2_PLACEMENT_3D ( 'NONE', #11332, #17588, #14602 ) ;
#11704 = EDGE_CURVE ( 'NONE', #8865, #383, #11639, .T. ) ;
#11705 = DIRECTION ( 'NONE',  ( 1.000000000000000000, 0.000000000000000000, 0.000000000000000000 ) ) ;
#11706 = AXIS2_PLACEMENT_3D ( 'NONE', #7028, #11621, #10095 ) ;
#11707 = FACE_BOUND ( 'NONE', #12840, .T. ) ;
#11708 = DIRECTION ( 'NONE',  ( -0.7071067811865516806, 0.000000000000000000, 0.7071067811865434649 ) ) ;
#11709 = ORIENTED_EDGE ( 'NONE', *, *, #9766, .T. ) ;
#11710 = DIRECTION ( 'NONE',  ( -0.000000000000000000, -0.000000000000000000, 1.000000000000000000 ) ) ;
#11711 = DIRECTION ( 'NONE',  ( 0.000000000000000000, 0.000000000000000000, 1.000000000000000000 ) ) ;
#11712 = ORIENTED_EDGE ( 'NONE', *, *, #5675, .T. ) ;
#11713 = FACE_OUTER_BOUND ( 'NONE', #7433, .T. ) ;
#11714 = CYLINDRICAL_SURFACE ( 'NONE', #10995, 17.50000000000000355 ) ;
#11715 = FACE_OUTER_BOUND ( 'NONE', #1785, .T. ) ;
#11716 = CARTESIAN_POINT ( 'NONE',  ( 67.36461649554532016, -39.84224160888924615, 110.9660488491357455 ) ) ;
#11717 = VECTOR ( 'NONE', #14658, 1000.000000000000227 ) ;
#11718 = ADVANCED_FACE ( 'NONE', ( #17600 ), #8114, .F. ) ;
#11719 = EDGE_CURVE ( 'NONE', #11007, #16337, #402, .T. ) ;
#11720 = DIRECTION ( 'NONE',  ( 0.000000000000000000, 0.000000000000000000, -1.000000000000000000 ) ) ;
#11721 = PLANE ( 'NONE',  #2835 ) ;
#11722 = VECTOR ( 'NONE', #4631, 1000.000000000000000 ) ;
#11723 = CIRCLE ( 'NONE', #307, 10.00000000000000888 ) ;
#11724 = VERTEX_POINT ( 'NONE', #6944 ) ;
#11725 = EDGE_CURVE ( 'NONE', #5887, #4216, #16164, .T. ) ;
#11726 = DIRECTION ( 'NONE',  ( 0.2080686897406943681, 0.9781142164131909622, 0.000000000000000000 ) ) ;
#11727 = ORIENTED_EDGE ( 'NONE', *, *, #15789, .T. ) ;
#11728 = EDGE_LOOP ( 'NONE', ( #19858, #5069, #14516 ) ) ;
#11729 = DIRECTION ( 'NONE',  ( 0.000000000000000000, 0.000000000000000000, -1.000000000000000000 ) ) ;
#11730 = ORIENTED_EDGE ( 'NONE', *, *, #11873, .T. ) ;
#11731 = ADVANCED_FACE ( 'NONE', ( #600 ), #3577, .F. ) ;
#11732 = FACE_OUTER_BOUND ( 'NONE', #16209, .T. ) ;
#11733 = DIRECTION ( 'NONE',  ( 0.000000000000000000, 0.000000000000000000, 1.000000000000000000 ) ) ;
#11734 = DIRECTION ( 'NONE',  ( 1.000000000000000000, 0.000000000000000000, 0.000000000000000000 ) ) ;
#11735 = DIRECTION ( 'NONE',  ( -1.000000000000000000, 0.000000000000000000, 0.000000000000000000 ) ) ;
#11736 = CIRCLE ( 'NONE', #13368, 7.500000000000007994 ) ;
#11737 = CIRCLE ( 'NONE', #16983, 62.91752772691707207 ) ;
#11738 = ORIENTED_EDGE ( 'NONE', *, *, #14526, .F. ) ;
#11739 = CARTESIAN_POINT ( 'NONE',  ( 0.000000000000000000, 0.000000000000000000, 283.5832628385307999 ) ) ;
#11740 = DIRECTION ( 'NONE',  ( 0.000000000000000000, 0.000000000000000000, 1.000000000000000000 ) ) ;
#11741 = LINE ( 'NONE', #3880, #344 ) ;
#11742 = DIRECTION ( 'NONE',  ( -0.000000000000000000, -0.000000000000000000, 1.000000000000000000 ) ) ;
#11743 = ORIENTED_EDGE ( 'NONE', *, *, #18025, .F. ) ;
#11744 = DIRECTION ( 'NONE',  ( -0.9271237148521547233, 0.3747554100459928872, 0.000000000000000000 ) ) ;
#11745 = ADVANCED_FACE ( 'NONE', ( #15957 ), #17703, .T. ) ;
#11746 = CYLINDRICAL_SURFACE ( 'NONE', #1978, 60.74260934110282051 ) ;
#11747 = CARTESIAN_POINT ( 'NONE',  ( 0.000000000000000000, 60.00000000000000000, -115.0000000000000000 ) ) ;
#11748 = VERTEX_POINT ( 'NONE', #3474 ) ;
#11749 = ADVANCED_FACE ( 'NONE', ( #8474 ), #6556, .T. ) ;
#11750 = DIRECTION ( 'NONE',  ( 0.000000000000000000, 0.000000000000000000, 1.000000000000000000 ) ) ;
#11751 = CARTESIAN_POINT ( 'NONE',  ( 28.06680738835026290, -53.87178215532764369, 293.5832628385307999 ) ) ;
#11752 = CIRCLE ( 'NONE', #16996, 3.224098631618459443 ) ;
#11753 = EDGE_LOOP ( 'NONE', ( #7144, #2867, #4920 ) ) ;
#11754 = AXIS2_PLACEMENT_3D ( 'NONE', #11763, #11857, #3804 ) ;
#11755 = ORIENTED_EDGE ( 'NONE', *, *, #660, .T. ) ;
#11756 = ORIENTED_EDGE ( 'NONE', *, *, #18359, .F. ) ;
#11757 = LINE ( 'NONE', #5631, #15678 ) ;
#11758 = ADVANCED_FACE ( 'NONE', ( #8068 ), #17500, .F. ) ;
#11759 = LINE ( 'NONE', #5737, #16560 ) ;
#11760 = ORIENTED_EDGE ( 'NONE', *, *, #14480, .F. ) ;
#11761 = CARTESIAN_POINT ( 'NONE',  ( 105.2664779077307884, -122.4188771607189636, 0.2361259031218233828 ) ) ;
#11762 = CARTESIAN_POINT ( 'NONE',  ( -99.35657680079187060, -131.4542451999402033, 4.193517943865902708 ) ) ;
#11763 = CARTESIAN_POINT ( 'NONE',  ( 144.1130761623740568, -69.50842595698583182, 10.00000000000000178 ) ) ;
#11764 = DIRECTION ( 'NONE',  ( 0.8660254037844380415, 0.5000000000000009992, 0.000000000000000000 ) ) ;
#11765 = DIRECTION ( 'NONE',  ( 0.000000000000000000, 0.000000000000000000, 1.000000000000000000 ) ) ;
#11766 = EDGE_CURVE ( 'NONE', #3444, #7406, #17966, .T. ) ;
#11767 = DIRECTION ( 'NONE',  ( -0.000000000000000000, -0.000000000000000000, -1.000000000000000000 ) ) ;
#11768 = CARTESIAN_POINT ( 'NONE',  ( 41.69438488732666315, 106.8146822993833780, 14.88498244535515980 ) ) ;
#11769 = EDGE_CURVE ( 'NONE', #14351, #3447, #701, .T. ) ;
#11770 = ORIENTED_EDGE ( 'NONE', *, *, #4787, .T. ) ;
#11771 = DIRECTION ( 'NONE',  ( 0.000000000000000000, 0.000000000000000000, 1.000000000000000000 ) ) ;
#11772 = DIRECTION ( 'NONE',  ( -0.2225209339563195554, 0.9749279121818223981, 0.000000000000000000 ) ) ;
#11773 = EDGE_CURVE ( 'NONE', #3116, #2014, #7185, .T. ) ;
#11774 = AXIS2_PLACEMENT_3D ( 'NONE', #8854, #10289, #13246 ) ;
#11775 = ORIENTED_EDGE ( 'NONE', *, *, #8019, .T. ) ;
#11776 =( NAMED_UNIT ( * ) SI_UNIT ( $, .STERADIAN. ) SOLID_ANGLE_UNIT ( ) );
#11777 = AXIS2_PLACEMENT_3D ( 'NONE', #4645, #13942, #2701 ) ;
#11778 = ORIENTED_EDGE ( 'NONE', *, *, #11500, .T. ) ;
#11779 = CARTESIAN_POINT ( 'NONE',  ( -110.0000000000000142, 285.0000000000000568, -67.49999999999997158 ) ) ;
#11780 = ORIENTED_EDGE ( 'NONE', *, *, #1653, .T. ) ;
#11781 = CARTESIAN_POINT ( 'NONE',  ( 134.2873401242900968, -76.10409495552309522, 4.733913478436992506 ) ) ;
#11782 = AXIS2_PLACEMENT_3D ( 'NONE', #6694, #2088, #447 ) ;
#11783 = CARTESIAN_POINT ( 'NONE',  ( -130.1925331961320751, -74.50863253846083012, -6.296416515224506405 ) ) ;
#11784 = CARTESIAN_POINT ( 'NONE',  ( 23.23469325536231622, -13.41455640552199924, 39.88498244535529125 ) ) ;
#11785 = PLANE ( 'NONE',  #10767 ) ;
#11786 = CARTESIAN_POINT ( 'NONE',  ( -27.49999999999998934, 0.000000000000000000, 43.88498244535566073 ) ) ;
#11787 = CARTESIAN_POINT ( 'NONE',  ( 159.9599531637113330, -36.50981547336952104, 39.99999999999999289 ) ) ;
#11788 = VECTOR ( 'NONE', #12784, 1000.000000000000000 ) ;
#11789 = CARTESIAN_POINT ( 'NONE',  ( 134.5816389422699899, -73.99824545063979997, 6.893745202855313003 ) ) ;
#11790 = CARTESIAN_POINT ( 'NONE',  ( 0.000000000000000000, 0.000000000000000000, 132.4711112102474146 ) ) ;
#11791 = AXIS2_PLACEMENT_3D ( 'NONE', #5162, #15797, #1876 ) ;
#11792 = LINE ( 'NONE', #18054, #6456 ) ;
#11793 = CARTESIAN_POINT ( 'NONE',  ( -133.1725405177978985, -69.15900471360698987, 32.12259856486934240 ) ) ;
#11794 = ORIENTED_EDGE ( 'NONE', *, *, #11395, .T. ) ;
#11795 = ORIENTED_EDGE ( 'NONE', *, *, #14653, .T. ) ;
#11796 = ORIENTED_EDGE ( 'NONE', *, *, #12108, .F. ) ;
#11797 = ORIENTED_EDGE ( 'NONE', *, *, #16504, .F. ) ;
#11798 = ORIENTED_EDGE ( 'NONE', *, *, #15585, .T. ) ;
#11799 = CARTESIAN_POINT ( 'NONE',  ( -49.07263256785926586, 39.37628763770471352, 248.9926560891072143 ) ) ;
#11800 = CARTESIAN_POINT ( 'NONE',  ( -51.77076963420847022, 31.77187437101487077, 283.5832628385307999 ) ) ;
#11801 = ORIENTED_EDGE ( 'NONE', *, *, #4132, .F. ) ;
#11802 = VECTOR ( 'NONE', #8633, 1000.000000000000000 ) ;
#11803 = CARTESIAN_POINT ( 'NONE',  ( -110.0000000000000142, 265.0000000000000000, -34.99999999999997868 ) ) ;
#11804 = CARTESIAN_POINT ( 'NONE',  ( -110.0000000000000142, 275.0000000000000000, 5.000000000000000888 ) ) ;
#11805 = ORIENTED_EDGE ( 'NONE', *, *, #12464, .T. ) ;
#11806 = DIRECTION ( 'NONE',  ( 0.9396926207859058744, 0.3420201433256757628, 0.000000000000000000 ) ) ;
#11807 = CARTESIAN_POINT ( 'NONE',  ( -1.396592535537253342E-14, 0.000000000000000000, 39.88498244535545467 ) ) ;
#11808 = CARTESIAN_POINT ( 'NONE',  ( -134.6712220124679220, -73.31159846691423354, 8.086032381974947114 ) ) ;
#11809 = DIRECTION ( 'NONE',  ( 0.000000000000000000, 0.000000000000000000, 1.000000000000000000 ) ) ;
#11810 = CARTESIAN_POINT ( 'NONE',  ( 128.4575182282473804, -77.52436737398417677, 40.44800108617082657 ) ) ;
#11811 = DIRECTION ( 'NONE',  ( 0.9993852124581887875, -0.03505990758545544927, 0.000000000000000000 ) ) ;
#11812 = ORIENTED_EDGE ( 'NONE', *, *, #17554, .T. ) ;
#11813 = EDGE_CURVE ( 'NONE', #1994, #6070, #3863, .T. ) ;
#11814 = LINE ( 'NONE', #11441, #5351 ) ;
#11815 = AXIS2_PLACEMENT_3D ( 'NONE', #8561, #11533, #16253 ) ;
#11816 = AXIS2_PLACEMENT_3D ( 'NONE', #9622, #14226, #15765 ) ;
#11817 = EDGE_LOOP ( 'NONE', ( #7627, #16927, #1267, #18561 ) ) ;
#11818 = ORIENTED_EDGE ( 'NONE', *, *, #18038, .F. ) ;
#11819 = DIRECTION ( 'NONE',  ( -1.000000000000000000, -0.000000000000000000, -0.000000000000000000 ) ) ;
#11820 = EDGE_LOOP ( 'NONE', ( #17571, #13767, #95, #10510, #7302, #813, #12418, #17596, #13557, #10848, #7552, #10187, #11701, #18900, #3869, #8118, #19582, #2240, #4014, #7682, #11656, #5776, #9621, #20070, #17451, #5203, #18589 ) ) ;
#11821 = ORIENTED_EDGE ( 'NONE', *, *, #11469, .T. ) ;
#11822 = VECTOR ( 'NONE', #16691, 1000.000000000000000 ) ;
#11823 = DIRECTION ( 'NONE',  ( -0.000000000000000000, -0.000000000000000000, 1.000000000000000000 ) ) ;
#11824 = EDGE_CURVE ( 'NONE', #9575, #14755, #5119, .T. ) ;
#11825 = CARTESIAN_POINT ( 'NONE',  ( -82.76227416097489709, -125.1020663115147755, 35.71415065638597497 ) ) ;
#11826 = PLANE ( 'NONE',  #12920 ) ;
#11827 = DIRECTION ( 'NONE',  ( 6.982962677686266711E-15, -0.000000000000000000, 1.000000000000000000 ) ) ;
#11828 = EDGE_CURVE ( 'NONE', #3875, #5457, #1242, .T. ) ;
#11829 = VERTEX_POINT ( 'NONE', #11922 ) ;
#11830 = CARTESIAN_POINT ( 'NONE',  ( 18.28567271940513450, -57.92709869106715814, 283.5832628385307999 ) ) ;
#11832 = CIRCLE ( 'NONE', #5650, 7.500000000000006217 ) ;
#11831 = CARTESIAN_POINT ( 'NONE',  ( 3.304959094393419949, 31.03941509555038181, 39.88498244535543336 ) ) ;
#11833 = VECTOR ( 'NONE', #15258, 1000.000000000000000 ) ;
#11834 = PLANE ( 'NONE',  #7522 ) ;
#11835 = FACE_OUTER_BOUND ( 'NONE', #9709, .T. ) ;
#11836 = ORIENTED_EDGE ( 'NONE', *, *, #18417, .F. ) ;
#11837 = DIRECTION ( 'NONE',  ( 1.000000000000000000, 0.000000000000000000, 0.000000000000000000 ) ) ;
#11838 = VECTOR ( 'NONE', #8472, 1000.000000000000000 ) ;
#11839 = CARTESIAN_POINT ( 'NONE',  ( -58.83691981461618781, 22.28973221005139749, 293.5832628385307999 ) ) ;
#11840 = DIRECTION ( 'NONE',  ( -0.1736481776669280275, 0.9848077530122084644, 1.076098267568195831E-15 ) ) ;
#11841 = ORIENTED_EDGE ( 'NONE', *, *, #401, .T. ) ;
#11842 = EDGE_CURVE ( 'NONE', #18228, #14365, #16461, .T. ) ;
#11843 = DIRECTION ( 'NONE',  ( 0.1390141521205946196, -0.9902903945359624593, 0.000000000000000000 ) ) ;
#11844 = CARTESIAN_POINT ( 'NONE',  ( -110.0000000000000142, 86.60254037844390496, 39.99999999999997868 ) ) ;
#11845 = AXIS2_PLACEMENT_3D ( 'NONE', #9096, #20048, #4710 ) ;
#11846 = EDGE_LOOP ( 'NONE', ( #14010, #13798, #8606 ) ) ;
#11847 = ORIENTED_EDGE ( 'NONE', *, *, #4247, .T. ) ;
#11848 = STYLED_ITEM ( 'NONE', ( #19159 ), #8063 ) ;
#11849 = FACE_OUTER_BOUND ( 'NONE', #14281, .T. ) ;
#11850 = EDGE_CURVE ( 'NONE', #14775, #5152, #15012, .T. ) ;
#11851 = PLANE ( 'NONE',  #11330 ) ;
#11852 = VERTEX_POINT ( 'NONE', #15205 ) ;
#11853 = EDGE_CURVE ( 'NONE', #19783, #14388, #2441, .T. ) ;
#11854 = CIRCLE ( 'NONE', #13172, 42.50000000000000000 ) ;
#11855 = DIRECTION ( 'NONE',  ( 0.000000000000000000, -1.000000000000000000, 3.338476886082577323E-16 ) ) ;
#11856 = CARTESIAN_POINT ( 'NONE',  ( -107.4999999999999716, -118.5063289449133777, -6.938893903907228378E-15 ) ) ;
#11857 = DIRECTION ( 'NONE',  ( -8.294538580027652572E-17, 2.273402209432136919E-16, -1.000000000000000000 ) ) ;
#11858 = DIRECTION ( 'NONE',  ( -0.000000000000000000, -0.000000000000000000, 1.000000000000000000 ) ) ;
#11859 = CARTESIAN_POINT ( 'NONE',  ( 87.50000000000005684, -133.9542832461881403, 30.00000000000000000 ) ) ;
#11860 = DIRECTION ( 'NONE',  ( -1.000000000000000000, 0.000000000000000000, 0.000000000000000000 ) ) ;
#11861 = CARTESIAN_POINT ( 'NONE',  ( -103.8888757476053541, -46.65403860089418941, 14.88498244535617765 ) ) ;
#11862 = ORIENTED_EDGE ( 'NONE', *, *, #12464, .F. ) ;
#11863 = ADVANCED_FACE ( 'NONE', ( #19710 ), #19812, .F. ) ;
#11864 = CARTESIAN_POINT ( 'NONE',  ( -1.607844166819003129E-13, 26.82911281104372847, 14.88498244535545112 ) ) ;
#11865 = CARTESIAN_POINT ( 'NONE',  ( 1.289614712049185874, -5.590028426173808462, 293.5832628385307999 ) ) ;
#11866 = VERTEX_POINT ( 'NONE', #5510 ) ;
#11867 = VECTOR ( 'NONE', #8705, 1000.000000000000000 ) ;
#11868 = VERTEX_POINT ( 'NONE', #8573 ) ;
#11869 = CIRCLE ( 'NONE', #8934, 60.74260934110282051 ) ;
#11870 = ORIENTED_EDGE ( 'NONE', *, *, #11164, .T. ) ;
#11871 = DIRECTION ( 'NONE',  ( -0.000000000000000000, -1.000000000000000000, -0.000000000000000000 ) ) ;
#11872 = ORIENTED_EDGE ( 'NONE', *, *, #10904, .T. ) ;
#11873 = EDGE_CURVE ( 'NONE', #2341, #8253, #994, .T. ) ;
#11874 = EDGE_CURVE ( 'NONE', #4820, #16400, #3548, .T. ) ;
#11875 = EDGE_CURVE ( 'NONE', #12652, #18954, #1190, .T. ) ;
#11876 = CARTESIAN_POINT ( 'NONE',  ( -60.00000000000000000, -2.094888803305880013E-13, -115.0000000000000000 ) ) ;
#11877 = DIRECTION ( 'NONE',  ( -0.000000000000000000, -0.000000000000000000, -1.000000000000000000 ) ) ;
#11878 = ADVANCED_FACE ( 'NONE', ( #17995 ), #12030, .T. ) ;
#11879 = ADVANCED_FACE ( 'NONE', ( #11732 ), #13563, .F. ) ;
#11880 = LINE ( 'NONE', #15164, #5930 ) ;
#11881 = CARTESIAN_POINT ( 'NONE',  ( -106.9434277526348183, -119.5160896407976736, 40.00000000000000711 ) ) ;
#11882 = AXIS2_PLACEMENT_3D ( 'NONE', #9522, #3286, #11456 ) ;
#11883 = CARTESIAN_POINT ( 'NONE',  ( 7.950000000000000178, 0.000000000000000000, 9.000000000000001776 ) ) ;
#11884 = ORIENTED_EDGE ( 'NONE', *, *, #7900, .F. ) ;
#11885 = CARTESIAN_POINT ( 'NONE',  ( 171.6840451157850111, -203.4275095296241318, 0.000000000000000000 ) ) ;
#11886 = CARTESIAN_POINT ( 'NONE',  ( 134.5432410141372941, -66.31847138156594212, 3.787490405755995937 ) ) ;
#11887 = VECTOR ( 'NONE', #14169, 1000.000000000000000 ) ;
#11888 = CYLINDRICAL_SURFACE ( 'NONE', #6913, 150.0000000000000284 ) ;
#11889 = LINE ( 'NONE', #10074, #12323 ) ;
#11890 = CARTESIAN_POINT ( 'NONE',  ( -132.8875376985349135, -69.70168330572197135, 33.61525977266834531 ) ) ;
#11891 = ORIENTED_EDGE ( 'NONE', *, *, #5156, .F. ) ;
#11892 = EDGE_CURVE ( 'NONE', #10368, #6110, #16617, .T. ) ;
#11893 = AXIS2_PLACEMENT_3D ( 'NONE', #16855, #9180, #9287 ) ;
#11894 = ORIENTED_EDGE ( 'NONE', *, *, #9024, .F. ) ;
#11895 = ORIENTED_EDGE ( 'NONE', *, *, #15760, .T. ) ;
#11896 = AXIS2_PLACEMENT_3D ( 'NONE', #12663, #11335, #15641 ) ;
#11897 = ORIENTED_EDGE ( 'NONE', *, *, #9095, .T. ) ;
#11898 = EDGE_LOOP ( 'NONE', ( #12674, #17483, #11992, #6893 ) ) ;
#11899 = ADVANCED_FACE ( 'NONE', ( #13460 ), #2743, .F. ) ;
#11900 = CARTESIAN_POINT ( 'NONE',  ( -136.4994460260996902, -31.11111111111111427, 27.86436879316430648 ) ) ;
#11901 = FACE_BOUND ( 'NONE', #15904, .T. ) ;
#11902 = DIRECTION ( 'NONE',  ( -0.000000000000000000, -0.000000000000000000, 1.000000000000000000 ) ) ;
#11903 = ORIENTED_EDGE ( 'NONE', *, *, #4921, .T. ) ;
#11905 = DIRECTION ( 'NONE',  ( -0.3420201433256630508, -0.9396926207859104263, 0.000000000000000000 ) ) ;
#11904 = AXIS2_PLACEMENT_3D ( 'NONE', #12137, #5713, #15317 ) ;
#11906 = CYLINDRICAL_SURFACE ( 'NONE', #10407, 112.8770930172170210 ) ;
#11907 = EDGE_CURVE ( 'NONE', #19329, #4788, #6820, .T. ) ;
#11908 = ORIENTED_EDGE ( 'NONE', *, *, #14125, .T. ) ;
#11909 = CARTESIAN_POINT ( 'NONE',  ( 7.950000000000000178, 7.347880794884121708E-16, -6.000000000000001776 ) ) ;
#11910 = DIRECTION ( 'NONE',  ( 1.000000000000000000, 0.000000000000000000, 0.000000000000000000 ) ) ;
#11911 = CARTESIAN_POINT ( 'NONE',  ( -133.9050245804181714, -78.55577302928912786, 3.168096144027441774 ) ) ;
#11912 = CIRCLE ( 'NONE', #15529, 7.500000000000007105 ) ;
#11913 = FACE_OUTER_BOUND ( 'NONE', #8334, .T. ) ;
#11914 = FACE_OUTER_BOUND ( 'NONE', #9504, .T. ) ;
#11915 = CARTESIAN_POINT ( 'NONE',  ( 49.24833719034187851, 60.83768308848395634, 110.7293897666001214 ) ) ;
#11916 = ORIENTED_EDGE ( 'NONE', *, *, #17334, .T. ) ;
#11917 = FACE_OUTER_BOUND ( 'NONE', #8341, .T. ) ;
#11918 = ORIENTED_EDGE ( 'NONE', *, *, #19716, .T. ) ;
#11919 = CARTESIAN_POINT ( 'NONE',  ( -58.03804081968160489, 8.833100819208169696, 132.4711112102474146 ) ) ;
#11920 = ORIENTED_EDGE ( 'NONE', *, *, #15775, .T. ) ;
#11921 = VERTEX_POINT ( 'NONE', #16655 ) ;
#11922 = CARTESIAN_POINT ( 'NONE',  ( 21.51662357878014831, -16.14275151819498078, 39.88498244535530546 ) ) ;
#11923 = SURFACE_SIDE_STYLE ('',( #17064 ) ) ;
#11924 = CARTESIAN_POINT ( 'NONE',  ( 0.5590800469813659301, 9.968355046870087222, 0.7343025909353927405 ) ) ;
#11925 = DIRECTION ( 'NONE',  ( 0.000000000000000000, 0.000000000000000000, -1.000000000000000000 ) ) ;
#11926 = DIRECTION ( 'NONE',  ( -0.9848077530122073542, -0.1736481776669340227, 0.000000000000000000 ) ) ;
#11927 = EDGE_CURVE ( 'NONE', #5660, #12327, #6543, .T. ) ;
#11928 = ORIENTED_EDGE ( 'NONE', *, *, #5881, .F. ) ;
#11929 = CARTESIAN_POINT ( 'NONE',  ( -163.5019688434124419, -20.99123081650240863, 60.00000000000000000 ) ) ;
#11930 = CYLINDRICAL_SURFACE ( 'NONE', #17609, 60.74260934110282051 ) ;
#11931 = FACE_OUTER_BOUND ( 'NONE', #1637, .T. ) ;
#11932 = AXIS2_PLACEMENT_3D ( 'NONE', #16783, #15341, #7565 ) ;
#11933 = DIRECTION ( 'NONE',  ( -0.9396926207859068736, -0.3420201433256725987, 0.000000000000000000 ) ) ;
#11934 = ORIENTED_EDGE ( 'NONE', *, *, #16862, .F. ) ;
#11935 = CARTESIAN_POINT ( 'NONE',  ( -189.9999999999988916, 275.0000000000000000, -2.499999999999734879 ) ) ;
#11936 = CARTESIAN_POINT ( 'NONE',  ( -132.8201933467846061, -84.36756360499408913, 39.04630981318919680 ) ) ;
#11937 = CARTESIAN_POINT ( 'NONE',  ( -76.92888220842476699, 14.39940464655786201, 112.0427633081292385 ) ) ;
#11938 = EDGE_LOOP ( 'NONE', ( #3645, #19614, #8406, #11517 ) ) ;
#11939 = EDGE_CURVE ( 'NONE', #13503, #8985, #19916, .T. ) ;
#11940 = DIRECTION ( 'NONE',  ( -6.982962677686267499E-15, -3.944304526105059027E-31, -1.000000000000000000 ) ) ;
#11941 = DIRECTION ( 'NONE',  ( -0.6427876096865456912, 0.7660444431189725734, -0.000000000000000000 ) ) ;
#11942 = ORIENTED_EDGE ( 'NONE', *, *, #13485, .T. ) ;
#11943 = AXIS2_PLACEMENT_3D ( 'NONE', #18266, #12313, #1066 ) ;
#11944 = VERTEX_POINT ( 'NONE', #10204 ) ;
#11945 = CARTESIAN_POINT ( 'NONE',  ( 7.500000000000420997, -60.00000000000000000, -115.0000000000000000 ) ) ;
#11946 = CIRCLE ( 'NONE', #17210, 150.0000000000000284 ) ;
#11947 = ORIENTED_EDGE ( 'NONE', *, *, #11813, .F. ) ;
#11948 = CARTESIAN_POINT ( 'NONE',  ( -9.176097008934114285, -25.21111933077039069, 14.88498244535551507 ) ) ;
#11949 = VECTOR ( 'NONE', #8756, 999.9999999999998863 ) ;
#11950 = CARTESIAN_POINT ( 'NONE',  ( 0.000000000000000000, 0.000000000000000000, 293.5832628385307999 ) ) ;
#11951 = EDGE_LOOP ( 'NONE', ( #9381, #2042, #18878, #3962 ) ) ;
#11952 = DIRECTION ( 'NONE',  ( -0.000000000000000000, -0.000000000000000000, 1.000000000000000000 ) ) ;
#11953 = CARTESIAN_POINT ( 'NONE',  ( -100.7812499999999716, -111.0996833858562951, -10.00000000000000533 ) ) ;
#11954 = EDGE_CURVE ( 'NONE', #5657, #19395, #8672, .T. ) ;
#11955 = ADVANCED_FACE ( 'NONE', ( #19617 ), #18598, .T. ) ;
#11956 = AXIS2_PLACEMENT_3D ( 'NONE', #5715, #6949, #16468 ) ;
#11957 = CARTESIAN_POINT ( 'NONE',  ( -79.05640494597938073, -127.4758205975444270, 49.99999999999999289 ) ) ;
#11958 = DIRECTION ( 'NONE',  ( 0.3088643371590125142, -0.9511061040868803440, 0.000000000000000000 ) ) ;
#11959 = CARTESIAN_POINT ( 'NONE',  ( 70.38703763562273252, -92.47916748300480094, 14.88498244535495907 ) ) ;
#11960 = VECTOR ( 'NONE', #5438, 1000.000000000000114 ) ;
#11961 = CARTESIAN_POINT ( 'NONE',  ( -44.43084819159250287, 38.35506425062501989, 110.7293897666001214 ) ) ;
#11962 = DIRECTION ( 'NONE',  ( -0.2080686897406943958, -0.9781142164131909622, 0.000000000000000000 ) ) ;
#11963 = DIRECTION ( 'NONE',  ( -0.6427876096865405842, 0.7660444431189771253, 0.000000000000000000 ) ) ;
#11964 = CARTESIAN_POINT ( 'NONE',  ( -19.23614321207234923, 57.61627707419557254, 283.5832628385307999 ) ) ;
#11965 = VERTEX_POINT ( 'NONE', #12443 ) ;
#11966 = VECTOR ( 'NONE', #4827, 1000.000000000000000 ) ;
#11967 = EDGE_CURVE ( 'NONE', #1270, #270, #16311, .T. ) ;
#11968 = DIRECTION ( 'NONE',  ( 1.000000000000000000, 0.000000000000000000, -0.000000000000000000 ) ) ;
#11969 = CARTESIAN_POINT ( 'NONE',  ( 57.61823435390807902, 19.23677882349220880, 293.5832628385307999 ) ) ;
#11970 = EDGE_CURVE ( 'NONE', #371, #16460, #609, .T. ) ;
#11971 = ORIENTED_EDGE ( 'NONE', *, *, #1033, .F. ) ;
#11972 = EDGE_CURVE ( 'NONE', #13146, #19269, #15305, .T. ) ;
#11973 = ORIENTED_EDGE ( 'NONE', *, *, #7033, .F. ) ;
#11974 =( NAMED_UNIT ( * ) PLANE_ANGLE_UNIT ( ) SI_UNIT ( $, .RADIAN. ) );
#11975 = ORIENTED_EDGE ( 'NONE', *, *, #5156, .T. ) ;
#11976 = CARTESIAN_POINT ( 'NONE',  ( -49.67518383744793908, 60.47951622432801599, 110.7293897666001214 ) ) ;
#11977 = ORIENTED_EDGE ( 'NONE', *, *, #508, .T. ) ;
#11978 = CARTESIAN_POINT ( 'NONE',  ( -97.59206265536077751, 66.04728469612305730, 14.88498244535613146 ) ) ;
#11979 = EDGE_CURVE ( 'NONE', #10259, #166, #3817, .T. ) ;
#11980 = AXIS2_PLACEMENT_3D ( 'NONE', #6442, #12664, #389 ) ;
#11981 = AXIS2_PLACEMENT_3D ( 'NONE', #18769, #4646, #4328 ) ;
#11982 = CARTESIAN_POINT ( 'NONE',  ( -97.52493780042978244, -113.9981091059117233, 37.52868439553851232 ) ) ;
#11983 = CYLINDRICAL_SURFACE ( 'NONE', #5118, 7.500000000000007105 ) ;
#11984 = DIRECTION ( 'NONE',  ( -0.9848077530122062440, -0.1736481776669404620, 0.000000000000000000 ) ) ;
#11985 = VERTEX_POINT ( 'NONE', #17170 ) ;
#11986 = DIRECTION ( 'NONE',  ( 0.000000000000000000, -1.000000000000000000, 0.000000000000000000 ) ) ;
#11987 = CARTESIAN_POINT ( 'NONE',  ( -134.9866372717062859, -65.41115948453617079, 7.014368073914691415 ) ) ;
#11988 = CARTESIAN_POINT ( 'NONE',  ( 132.1020537416659693, -71.17237643005199743, 3.900420950673862741 ) ) ;
#11989 = CARTESIAN_POINT ( 'NONE',  ( 0.000000000000000000, 0.000000000000000000, 0.000000000000000000 ) ) ;
#11990 = PLANE ( 'NONE',  #9727 ) ;
#11991 = CARTESIAN_POINT ( 'NONE',  ( -134.6257061167729603, -73.66332987390026688, 32.57991584872674196 ) ) ;
#11992 = ORIENTED_EDGE ( 'NONE', *, *, #17752, .F. ) ;
#11993 = CARTESIAN_POINT ( 'NONE',  ( -74.01264520835137262, 25.47058595421627913, 132.4711112102474146 ) ) ;
#11994 = EDGE_CURVE ( 'NONE', #15923, #12841, #18924, .T. ) ;
#11995 = AXIS2_PLACEMENT_3D ( 'NONE', #13565, #5812, #12031 ) ;
#11996 = ADVANCED_FACE ( 'NONE', ( #1305, #7943, #17272, #7538, #11010, #4470, #20224, #176 ), #18703, .T. ) ;
#11997 = EDGE_CURVE ( 'NONE', #17740, #16088, #15524, .T. ) ;
#11999 = ORIENTED_EDGE ( 'NONE', *, *, #8638, .T. ) ;
#11998 = AXIS2_PLACEMENT_3D ( 'NONE', #16896, #4412, #9215 ) ;
#12000 = ORIENTED_EDGE ( 'NONE', *, *, #12516, .T. ) ;
#12001 = ORIENTED_EDGE ( 'NONE', *, *, #11250, .F. ) ;
#12002 = VERTEX_POINT ( 'NONE', #7740 ) ;
#12003 = CARTESIAN_POINT ( 'NONE',  ( -136.9392167837085310, -29.18162474279422725, 27.35468135938761591 ) ) ;
#12004 = ADVANCED_FACE ( 'NONE', ( #20018 ), #12649, .T. ) ;
#12005 = CARTESIAN_POINT ( 'NONE',  ( -32.16802499836779106, -54.07248341783242296, 132.4711112102474146 ) ) ;
#12006 = DIRECTION ( 'NONE',  ( -0.000000000000000000, -0.000000000000000000, 1.000000000000000000 ) ) ;
#12007 = ORIENTED_EDGE ( 'NONE', *, *, #19765, .F. ) ;
#12008 = CARTESIAN_POINT ( 'NONE',  ( -139.0264712516304826, -13.50756410634541993, -14.56951644170016458 ) ) ;
#12009 = DIRECTION ( 'NONE',  ( 1.000000000000000000, 0.000000000000000000, 0.000000000000000000 ) ) ;
#12010 = CIRCLE ( 'NONE', #13306, 150.0000000000000284 ) ;
#12011 = ORIENTED_EDGE ( 'NONE', *, *, #6188, .F. ) ;
#12012 = DIRECTION ( 'NONE',  ( -0.6692498792541753394, -0.7430374143461900838, 0.000000000000000000 ) ) ;
#12013 = AXIS2_PLACEMENT_3D ( 'NONE', #10723, #6138, #16975 ) ;
#12014 = DIRECTION ( 'NONE',  ( -0.000000000000000000, -0.000000000000000000, 1.000000000000000000 ) ) ;
#12015 = CARTESIAN_POINT ( 'NONE',  ( 0.000000000000000000, 0.000000000000000000, 60.00000000000000000 ) ) ;
#12016 = CYLINDRICAL_SURFACE ( 'NONE', #1682, 7.500000000000000000 ) ;
#12017 = EDGE_CURVE ( 'NONE', #6230, #18743, #18909, .T. ) ;
#12018 = LINE ( 'NONE', #16548, #15955 ) ;
#12019 = CARTESIAN_POINT ( 'NONE',  ( -101.6421356237309226, -200.0000000000000000, 3.469446951953614189E-15 ) ) ;
#12020 = VERTEX_POINT ( 'NONE', #6328 ) ;
#12021 = DIRECTION ( 'NONE',  ( -6.982962677686266711E-15, 0.000000000000000000, -1.000000000000000000 ) ) ;
#12022 = AXIS2_PLACEMENT_3D ( 'NONE', #7841, #4687, #20119 ) ;
#12023 = ORIENTED_EDGE ( 'NONE', *, *, #6161, .T. ) ;
#12024 = CIRCLE ( 'NONE', #14329, 7.500000000000003553 ) ;
#12025 = EDGE_CURVE ( 'NONE', #3088, #7939, #1261, .T. ) ;
#12026 = ORIENTED_EDGE ( 'NONE', *, *, #18508, .F. ) ;
#12027 = CARTESIAN_POINT ( 'NONE',  ( -17.50000000000001776, 2.143131898507872981E-15, 39.88498244535557546 ) ) ;
#12028 = VERTEX_POINT ( 'NONE', #18490 ) ;
#12029 = ORIENTED_EDGE ( 'NONE', *, *, #16350, .T. ) ;
#12030 = PLANE ( 'NONE',  #17607 ) ;
#12031 = DIRECTION ( 'NONE',  ( 1.000000000000000000, 0.000000000000000000, 0.000000000000000000 ) ) ;
#12032 = EDGE_LOOP ( 'NONE', ( #2311, #13209, #7635, #3518 ) ) ;
#12033 = CARTESIAN_POINT ( 'NONE',  ( -62.90240729679781850, -1.379293853801974779, 132.4711112102474146 ) ) ;
#12034 = ORIENTED_EDGE ( 'NONE', *, *, #8577, .T. ) ;
#12035 = CARTESIAN_POINT ( 'NONE',  ( -131.0911649403506658, -72.90709374210203464, 45.08599941119474863 ) ) ;
#12036 = DIRECTION ( 'NONE',  ( 1.000000000000000000, 0.000000000000000000, 0.000000000000000000 ) ) ;
#12037 = CIRCLE ( 'NONE', #4183, 17.50000000000000355 ) ;
#12038 = AXIS2_PLACEMENT_3D ( 'NONE', #12451, #11623, #2231 ) ;
#12039 = DIRECTION ( 'NONE',  ( 0.000000000000000000, 0.000000000000000000, 1.000000000000000000 ) ) ;
#12040 = AXIS2_PLACEMENT_3D ( 'NONE', #1257, #13939, #8925 ) ;
#12041 = ORIENTED_EDGE ( 'NONE', *, *, #2613, .F. ) ;
#12042 = DIRECTION ( 'NONE',  ( 1.000000000000000000, 0.000000000000000000, 0.000000000000000000 ) ) ;
#12043 = CARTESIAN_POINT ( 'NONE',  ( -189.9999999999988916, 275.0000000000000000, 12.50000000000027178 ) ) ;
#12044 = FACE_OUTER_BOUND ( 'NONE', #118, .T. ) ;
#12045 = VERTEX_POINT ( 'NONE', #15420 ) ;
#12046 = CYLINDRICAL_SURFACE ( 'NONE', #6825, 10.00000000000000888 ) ;
#12047 = CARTESIAN_POINT ( 'NONE',  ( 0.000000000000000000, 0.000000000000000000, 283.5832628385307999 ) ) ;
#12048 = ORIENTED_EDGE ( 'NONE', *, *, #20022, .T. ) ;
#12049 = ORIENTED_EDGE ( 'NONE', *, *, #12363, .T. ) ;
#12050 = CARTESIAN_POINT ( 'NONE',  ( -97.49999999999997158, -133.9542832461881972, 30.00000000000000711 ) ) ;
#12051 = ORIENTED_EDGE ( 'NONE', *, *, #18427, .F. ) ;
#12052 = VECTOR ( 'NONE', #19192, 1000.000000000000000 ) ;
#12053 = VECTOR ( 'NONE', #8553, 1000.000000000000114 ) ;
#12054 = LINE ( 'NONE', #13699, #7818 ) ;
#12055 = DIRECTION ( 'NONE',  ( -0.6427876096865456912, 0.7660444431189726844, 0.000000000000000000 ) ) ;
#12056 = ORIENTED_EDGE ( 'NONE', *, *, #13598, .T. ) ;
#12057 = CARTESIAN_POINT ( 'NONE',  ( 95.49511753039645612, -115.9200926447949627, 6.565580923201594921 ) ) ;
#12058 = CARTESIAN_POINT ( 'NONE',  ( -99.34007343275230539, -112.3954413154799710, 0.8360693818916272724 ) ) ;
#12059 = DIRECTION ( 'NONE',  ( -0.4999999999999888978, -0.8660254037844449249, 0.000000000000000000 ) ) ;
#12060 = PLANE ( 'NONE',  #6582 ) ;
#12061 = CARTESIAN_POINT ( 'NONE',  ( 4.196299268919053915, 3.911853314815666671, 283.5832628385307999 ) ) ;
#12062 = CARTESIAN_POINT ( 'NONE',  ( 122.8001410695374602, -86.14014948502067170, -10.00000000000000178 ) ) ;
#12063 = CARTESIAN_POINT ( 'NONE',  ( 0.8038475772933556529, -5.196152422706607155, 8.999999999999998224 ) ) ;
#12064 = CARTESIAN_POINT ( 'NONE',  ( -67.50000000000000000, -2.085703952312275003E-13, -105.0000000000000142 ) ) ;
#12065 = FACE_OUTER_BOUND ( 'NONE', #10232, .T. ) ;
#12066 = EDGE_LOOP ( 'NONE', ( #5909, #15657, #6741, #9139, #556, #4110 ) ) ;
#12067 = CARTESIAN_POINT ( 'NONE',  ( -27.53920554013687649, -73.25972925305620720, 132.4711112102474146 ) ) ;
#12068 = CARTESIAN_POINT ( 'NONE',  ( -156.4179374840092862, -52.02840013024096066, 60.00000000000000000 ) ) ;
#12069 = ORIENTED_EDGE ( 'NONE', *, *, #1484, .T. ) ;
#12070 = EDGE_CURVE ( 'NONE', #14186, #10466, #10596, .T. ) ;
#12071 = ORIENTED_EDGE ( 'NONE', *, *, #16107, .T. ) ;
#12072 =( LENGTH_UNIT ( ) NAMED_UNIT ( * ) SI_UNIT ( .MILLI., .METRE. ) );
#12073 = ORIENTED_EDGE ( 'NONE', *, *, #8771, .T. ) ;
#12074 = FACE_BOUND ( 'NONE', #13068, .T. ) ;
#12075 = PRODUCT_DEFINITION_FORMATION_WITH_SPECIFIED_SOURCE ( 'ANY', '', #3622, .NOT_KNOWN. ) ;
#12076 = ORIENTED_EDGE ( 'NONE', *, *, #14588, .T. ) ;
#12077 = VECTOR ( 'NONE', #2904, 1000.000000000000000 ) ;
#12078 = PLANE ( 'NONE',  #9241 ) ;
#12079 = LINE ( 'NONE', #3409, #5029 ) ;
#12080 = FACE_OUTER_BOUND ( 'NONE', #5281, .T. ) ;
#12081 = EDGE_CURVE ( 'NONE', #10931, #13585, #16851, .T. ) ;
#12082 = CARTESIAN_POINT ( 'NONE',  ( 130.9868171408399462, -91.88282611735539263, -10.00000000000000000 ) ) ;
#12083 = EDGE_CURVE ( 'NONE', #4164, #347, #6120, .T. ) ;
#12084 = CARTESIAN_POINT ( 'NONE',  ( -19.30071112029641967, 55.43188410062188609, 248.9926560891072143 ) ) ;
#12085 = EDGE_LOOP ( 'NONE', ( #15156, #7980 ) ) ;
#12086 = EDGE_CURVE ( 'NONE', #1114, #17034, #15474, .T. ) ;
#12087 = DIRECTION ( 'NONE',  ( -0.000000000000000000, -0.000000000000000000, 1.000000000000000000 ) ) ;
#12088 = CARTESIAN_POINT ( 'NONE',  ( -134.7188131032835940, -72.93593548674768101, 9.625079458299000024 ) ) ;
#12089 = CARTESIAN_POINT ( 'NONE',  ( 132.0512179319785844, -87.77725330521087699, 0.2892730586186746389 ) ) ;
#12090 = CARTESIAN_POINT ( 'NONE',  ( -30.25670013172253192, -55.16472960512360402, 293.5832628385307999 ) ) ;
#12091 = DIRECTION ( 'NONE',  ( 0.1390141521205912056, -0.9902903945359629034, 0.000000000000000000 ) ) ;
#12092 = DIRECTION ( 'NONE',  ( -1.000000000000000000, 0.000000000000000000, 0.000000000000000000 ) ) ;
#12093 = VERTEX_POINT ( 'NONE', #13828 ) ;
#12094 = AXIS2_PLACEMENT_3D ( 'NONE', #10430, #12168, #16888 ) ;
#12095 = DIRECTION ( 'NONE',  ( -0.000000000000000000, 0.000000000000000000, -1.000000000000000000 ) ) ;
#12096 = CONICAL_SURFACE ( 'NONE', #17360, 17.50000000000001066, 0.7853981633974479459 ) ;
#12097 = EDGE_CURVE ( 'NONE', #9886, #7766, #18342, .T. ) ;
#12098 = VERTEX_POINT ( 'NONE', #16705 ) ;
#12099 = ORIENTED_EDGE ( 'NONE', *, *, #430, .F. ) ;
#12100 = ORIENTED_EDGE ( 'NONE', *, *, #14549, .T. ) ;
#12101 = EDGE_LOOP ( 'NONE', ( #9377, #3099, #9907, #5891 ) ) ;
#12102 = CARTESIAN_POINT ( 'NONE',  ( -138.4878096489830170, -24.82274991483212290, 25.33558894580708198 ) ) ;
#12103 = VECTOR ( 'NONE', #19136, 1000.000000000000000 ) ;
#12104 = LINE ( 'NONE', #18161, #475 ) ;
#12105 = EDGE_CURVE ( 'NONE', #13503, #1969, #4115, .T. ) ;
#12106 = CARTESIAN_POINT ( 'NONE',  ( -79.75827554147308263, 9.767571684737763671E-15, 293.5832628385307999 ) ) ;
#12107 = ORIENTED_EDGE ( 'NONE', *, *, #5993, .F. ) ;
#12108 = EDGE_CURVE ( 'NONE', #6717, #11659, #18546, .T. ) ;
#12109 = AXIS2_PLACEMENT_3D ( 'NONE', #16324, #2405, #856 ) ;
#12110 = DIRECTION ( 'NONE',  ( -0.5742676632334706710, 0.8186676071302499968, -0.000000000000000000 ) ) ;
#12111 = LINE ( 'NONE', #18370, #12053 ) ;
#12112 = ADVANCED_FACE ( 'NONE', ( #16605 ), #10550, .F. ) ;
#12113 = ORIENTED_EDGE ( 'NONE', *, *, #14110, .T. ) ;
#12114 = CARTESIAN_POINT ( 'NONE',  ( 116.5881606921955864, -25.59923667990641150, 39.88498244535464465 ) ) ;
#12115 = CARTESIAN_POINT ( 'NONE',  ( 23.22641211976289100, 56.12662799072080588, 283.5832628385307999 ) ) ;
#12116 = CARTESIAN_POINT ( 'NONE',  ( -132.1955596402976028, -87.17962382538664201, 0.3691654002908723586 ) ) ;
#12117 = CARTESIAN_POINT ( 'NONE',  ( 69.11703934647950121, -95.44259730872654757, 14.88498244535496973 ) ) ;
#12118 = UNCERTAINTY_MEASURE_WITH_UNIT (LENGTH_MEASURE( 1.000000000000000082E-05 ), #18810, 'distance_accuracy_value', 'NONE');
#12119 = DIRECTION ( 'NONE',  ( 1.000000000000000000, 0.000000000000000000, 0.000000000000000000 ) ) ;
#12120 = CARTESIAN_POINT ( 'NONE',  ( -174.2942412179009466, -197.9050378206823382, 40.00000000000000000 ) ) ;
#12121 = ORIENTED_EDGE ( 'NONE', *, *, #3755, .T. ) ;
#12122 = VERTEX_POINT ( 'NONE', #4218 ) ;
#12123 = EDGE_CURVE ( 'NONE', #9378, #8067, #9125, .T. ) ;
#12124 = CARTESIAN_POINT ( 'NONE',  ( 45.46712722958809394, -40.27908801170008246, 293.5832628385307999 ) ) ;
#12125 = EDGE_LOOP ( 'NONE', ( #19808, #16308, #9780, #9840 ) ) ;
#12126 = ORIENTED_EDGE ( 'NONE', *, *, #14997, .T. ) ;
#12127 = DIRECTION ( 'NONE',  ( 0.000000000000000000, 0.000000000000000000, 1.000000000000000000 ) ) ;
#12128 = VERTEX_POINT ( 'NONE', #1461 ) ;
#12129 = ORIENTED_EDGE ( 'NONE', *, *, #15135, .F. ) ;
#12130 = DIRECTION ( 'NONE',  ( 0.000000000000000000, 0.000000000000000000, 1.000000000000000000 ) ) ;
#12131 = CARTESIAN_POINT ( 'NONE',  ( -27.10287801637851501, 1.507547295587399638, 39.88498244535563941 ) ) ;
#12132 = DIRECTION ( 'NONE',  ( 0.000000000000000000, 0.000000000000000000, 1.000000000000000000 ) ) ;
#12133 = ORIENTED_EDGE ( 'NONE', *, *, #13591, .T. ) ;
#12134 = EDGE_CURVE ( 'NONE', #18587, #15066, #4424, .T. ) ;
#12135 = EDGE_CURVE ( 'NONE', #9853, #10824, #15368, .T. ) ;
#12136 = DIRECTION ( 'NONE',  ( -0.000000000000000000, -0.000000000000000000, -1.000000000000000000 ) ) ;
#12137 = CARTESIAN_POINT ( 'NONE',  ( 0.000000000000000000, 60.00000000000000000, -105.0000000000000142 ) ) ;
#12138 = ADVANCED_FACE ( 'NONE', ( #19918 ), #4472, .T. ) ;
#12139 = VERTEX_POINT ( 'NONE', #18600 ) ;
#12140 = DIRECTION ( 'NONE',  ( -0.7881095627315599650, -0.6155349844899714595, 0.000000000000000000 ) ) ;
#12141 = CARTESIAN_POINT ( 'NONE',  ( 152.4599531637113330, -36.50981547336952104, 39.99999999999999289 ) ) ;
#12142 = DIRECTION ( 'NONE',  ( -0.7660444431189813441, 0.6427876096865353661, 0.000000000000000000 ) ) ;
#12143 = ORIENTED_EDGE ( 'NONE', *, *, #17181, .F. ) ;
#12144 = CIRCLE ( 'NONE', #11815, 112.8770930172170210 ) ;
#12145 = VECTOR ( 'NONE', #12932, 1000.000000000000000 ) ;
#12146 = LINE ( 'NONE', #18406, #16908 ) ;
#12147 = DIRECTION ( 'NONE',  ( 1.000000000000000000, 0.000000000000000000, 0.000000000000000000 ) ) ;
#12148 = CARTESIAN_POINT ( 'NONE',  ( -107.8696296321708843, 89.24609338212388820, 39.93925132900347563 ) ) ;
#12149 = VERTEX_POINT ( 'NONE', #15208 ) ;
#12150 = DIRECTION ( 'NONE',  ( -6.982962677686266711E-15, 0.000000000000000000, -1.000000000000000000 ) ) ;
#12151 = DIRECTION ( 'NONE',  ( -0.3427509529624101492, 0.9394263059140720573, 0.000000000000000000 ) ) ;
#12152 = ORIENTED_EDGE ( 'NONE', *, *, #5127, .F. ) ;
#12153 = AXIS2_PLACEMENT_3D ( 'NONE', #8981, #14099, #10717 ) ;
#12154 = AXIS2_PLACEMENT_3D ( 'NONE', #14022, #16998, #7570 ) ;
#12155 = ORIENTED_EDGE ( 'NONE', *, *, #19219, .T. ) ;
#12156 = CARTESIAN_POINT ( 'NONE',  ( -82.07017599500312599, -125.5567397147592743, 31.48836724268550569 ) ) ;
#12157 = ORIENTED_EDGE ( 'NONE', *, *, #13531, .T. ) ;
#12158 = PLANE ( 'NONE',  #18280 ) ;
#12159 = CARTESIAN_POINT ( 'NONE',  ( 60.68773558783009747, -2.629322876227576433, 293.5832628385307999 ) ) ;
#12160 = CIRCLE ( 'NONE', #17427, 62.91752772691707207 ) ;
#12161 = ORIENTED_EDGE ( 'NONE', *, *, #15502, .T. ) ;
#12162 = AXIS2_PLACEMENT_3D ( 'NONE', #8806, #6056, #9002 ) ;
#12163 = LINE ( 'NONE', #5125, #2158 ) ;
#12164 = CARTESIAN_POINT ( 'NONE',  ( 53.40063514825077107, 28.94886449118924432, 283.5832628385307999 ) ) ;
#12165 = AXIS2_PLACEMENT_3D ( 'NONE', #9910, #888, #2340 ) ;
#12166 = EDGE_CURVE ( 'NONE', #19334, #9872, #17584, .T. ) ;
#12167 = LINE ( 'NONE', #2775, #7846 ) ;
#12168 = DIRECTION ( 'NONE',  ( 0.000000000000000000, 0.000000000000000000, 1.000000000000000000 ) ) ;
#12169 = DIRECTION ( 'NONE',  ( 1.000000000000000000, 0.000000000000000000, 0.000000000000000000 ) ) ;
#12170 = DIRECTION ( 'NONE',  ( -1.000000000000000000, 0.000000000000000000, -0.000000000000000000 ) ) ;
#12171 = DIRECTION ( 'NONE',  ( -0.000000000000000000, -0.000000000000000000, 1.000000000000000000 ) ) ;
#12172 = DIRECTION ( 'NONE',  ( -0.000000000000000000, -0.000000000000000000, 1.000000000000000000 ) ) ;
#12173 = CARTESIAN_POINT ( 'NONE',  ( 98.61625419099860324, -132.4696700755205256, 34.60511644944756426 ) ) ;
#12174 = VERTEX_POINT ( 'NONE', #19815 ) ;
#12175 = CARTESIAN_POINT ( 'NONE',  ( -1.629937663769596368, -60.72279549541552512, 293.5832628385307999 ) ) ;
#12176 = DIRECTION ( 'NONE',  ( 1.000000000000000000, 0.000000000000000000, 0.000000000000000000 ) ) ;
#12177 = VECTOR ( 'NONE', #696, 1000.000000000000227 ) ;
#12178 = AXIS2_PLACEMENT_3D ( 'NONE', #17712, #6955, #8385 ) ;
#12179 = ORIENTED_EDGE ( 'NONE', *, *, #8132, .F. ) ;
#12180 = VERTEX_POINT ( 'NONE', #6122 ) ;
#12181 = CIRCLE ( 'NONE', #746, 6.000000000000001776 ) ;
#12182 = ORIENTED_EDGE ( 'NONE', *, *, #18681, .T. ) ;
#12183 = FACE_BOUND ( 'NONE', #11577, .T. ) ;
#12184 = VECTOR ( 'NONE', #19838, 1000.000000000000000 ) ;
#12185 = VERTEX_POINT ( 'NONE', #2646 ) ;
#12186 = DIRECTION ( 'NONE',  ( 0.4693298356057531984, -0.8830229359480288309, 0.000000000000000000 ) ) ;
#12187 = CARTESIAN_POINT ( 'NONE',  ( 134.7188131032333729, -72.93593548660996362, 9.503255316708910883 ) ) ;
#12188 = DIRECTION ( 'NONE',  ( -0.000000000000000000, -0.000000000000000000, 1.000000000000000000 ) ) ;
#12189 = LINE ( 'NONE', #13415, #12785 ) ;
#12190 = AXIS2_PLACEMENT_3D ( 'NONE', #9932, #15031, #16181 ) ;
#12191 = CARTESIAN_POINT ( 'NONE',  ( -141.6227766016837961, -18.73072656238141320, -9.999999999999985789 ) ) ;
#12192 = DIRECTION ( 'NONE',  ( -0.7818314824680221431, -0.6234898018587431423, -0.000000000000000000 ) ) ;
#12193 = EDGE_CURVE ( 'NONE', #5152, #3741, #10597, .T. ) ;
#12194 = ORIENTED_EDGE ( 'NONE', *, *, #11997, .F. ) ;
#12195 = CARTESIAN_POINT ( 'NONE',  ( -159.9599531637108782, -36.50981547337168109, 39.99999999999999289 ) ) ;
#12196 = CYLINDRICAL_SURFACE ( 'NONE', #8022, 60.74260934110282051 ) ;
#12197 = CARTESIAN_POINT ( 'NONE',  ( 127.3242258594541880, -79.35722205891387659, -0.8910983717930788250 ) ) ;
#12198 = VECTOR ( 'NONE', #9857, 1000.000000000000000 ) ;
#12199 = DIRECTION ( 'NONE',  ( -6.982962677686266711E-15, 0.000000000000000000, -1.000000000000000000 ) ) ;
#12200 = CARTESIAN_POINT ( 'NONE',  ( 60.47951622432751151, 49.67518383744852883, 248.9926560891072143 ) ) ;
#12201 = CARTESIAN_POINT ( 'NONE',  ( -134.7188131035389063, -72.93593548744735244, 30.76221486496924129 ) ) ;
#12202 = ORIENTED_EDGE ( 'NONE', *, *, #18418, .T. ) ;
#12203 = CARTESIAN_POINT ( 'NONE',  ( -107.4999999999999716, -200.0000000000000000, 0.000000000000000000 ) ) ;
#12204 = COLOUR_RGB ( '', 0.31764706, 0.68627451, 0.89019608) ;
#12205 = EDGE_CURVE ( 'NONE', #345, #13281, #15261, .T. ) ;
#12206 = AXIS2_PLACEMENT_3D ( 'NONE', #3188, #18952, #9822 ) ;
#12207 = EDGE_LOOP ( 'NONE', ( #13180, #20194, #1707, #9065 ) ) ;
#12208 = ORIENTED_EDGE ( 'NONE', *, *, #15528, .F. ) ;
#12209 = EDGE_LOOP ( 'NONE', ( #9316, #9702, #18912, #13332 ) ) ;
#12210 = AXIS2_PLACEMENT_3D ( 'NONE', #9838, #2080, #8305 ) ;
#12211 = CARTESIAN_POINT ( 'NONE',  ( -141.0318087585327476, -19.69042926485499478, 21.20820817219406251 ) ) ;
#12212 = DIRECTION ( 'NONE',  ( -0.000000000000000000, -0.000000000000000000, 1.000000000000000000 ) ) ;
#12213 = CIRCLE ( 'NONE', #11247, 60.74260934110282051 ) ;
#12214 = CARTESIAN_POINT ( 'NONE',  ( 7.350000000000000533, -5.196152422706636465, -8.999999999999998224 ) ) ;
#12215 = ORIENTED_EDGE ( 'NONE', *, *, #592, .T. ) ;
#12216 = CARTESIAN_POINT ( 'NONE',  ( -136.4054103849693149, -26.47474353714355999, -17.99508669766643365 ) ) ;
#12217 = LINE ( 'NONE', #1490, #320 ) ;
#12218 = EDGE_CURVE ( 'NONE', #9259, #1807, #12990, .T. ) ;
#12219 = EDGE_LOOP ( 'NONE', ( #4260, #20038, #15939, #9806 ) ) ;
#12220 = CARTESIAN_POINT ( 'NONE',  ( -91.05432085726285152, 101.4279772787430574, -24.43173415096923407 ) ) ;
#12221 = CARTESIAN_POINT ( 'NONE',  ( -17.50000000000001066, 2.143131898507869431E-15, 83.57543755549745867 ) ) ;
#12222 = DIRECTION ( 'NONE',  ( 0.9009688679024154823, 0.4338837391175657809, 0.000000000000000000 ) ) ;
#12223 = CARTESIAN_POINT ( 'NONE',  ( 49.07263256785952166, -39.37628763770437956, 293.5832628385307999 ) ) ;
#12224 = CARTESIAN_POINT ( 'NONE',  ( 51.77251465595239921, -31.77296517111717478, 293.5832628385307999 ) ) ;
#12225 = CIRCLE ( 'NONE', #6043, 60.74260934110282051 ) ;
#12226 = CARTESIAN_POINT ( 'NONE',  ( 20.21777810286675958, 59.58067424803633116, 293.5832628385307999 ) ) ;
#12227 = ORIENTED_EDGE ( 'NONE', *, *, #6373, .T. ) ;
#12228 = ORIENTED_EDGE ( 'NONE', *, *, #11828, .T. ) ;
#12229 = ADVANCED_FACE ( 'NONE', ( #4581 ), #10808, .T. ) ;
#12230 = FACE_OUTER_BOUND ( 'NONE', #16792, .T. ) ;
#12231 = EDGE_LOOP ( 'NONE', ( #1756, #7112 ) ) ;
#12232 = EDGE_LOOP ( 'NONE', ( #5339, #5558, #9167, #18151 ) ) ;
#12233 = EDGE_CURVE ( 'NONE', #10391, #4654, #7742, .T. ) ;
#12234 = LINE ( 'NONE', #7633, #5017 ) ;
#12235 = ORIENTED_EDGE ( 'NONE', *, *, #13900, .F. ) ;
#12236 = ORIENTED_EDGE ( 'NONE', *, *, #4161, .T. ) ;
#12237 = CARTESIAN_POINT ( 'NONE',  ( 0.5590800469813547169, -5.620102221249795527, 8.265697409064612700 ) ) ;
#12238 = DIRECTION ( 'NONE',  ( 0.3427509529624101492, -0.9394263059140721683, 0.000000000000000000 ) ) ;
#12239 = CARTESIAN_POINT ( 'NONE',  ( 21.51741588379836756, 55.08582882688782689, 248.9926560891072143 ) ) ;
#12240 = EDGE_LOOP ( 'NONE', ( #8238, #5600, #2060, #14237 ) ) ;
#12241 = CIRCLE ( 'NONE', #8967, 79.75827554147308263 ) ;
#12242 = CARTESIAN_POINT ( 'NONE',  ( -2.629322876227788264, -60.68773558783006905, 293.5832628385307999 ) ) ;
#12243 = DIRECTION ( 'NONE',  ( 1.000000000000000000, 0.000000000000000000, -0.000000000000000000 ) ) ;
#12244 = ORIENTED_EDGE ( 'NONE', *, *, #8393, .T. ) ;
#12245 = EDGE_CURVE ( 'NONE', #3122, #15949, #20179, .T. ) ;
#12246 = CARTESIAN_POINT ( 'NONE',  ( -23.22718332831480481, -56.12853591711337486, 293.5832628385307999 ) ) ;
#12247 = FACE_OUTER_BOUND ( 'NONE', #18697, .T. ) ;
#12248 = CARTESIAN_POINT ( 'NONE',  ( 21.36933070621763164, -54.67896814532648619, 132.4711112102474146 ) ) ;
#12249 = DIRECTION ( 'NONE',  ( 1.000000000000000000, 0.000000000000000000, -6.994638739193269649E-15 ) ) ;
#12250 = CARTESIAN_POINT ( 'NONE',  ( -134.0425641885189805, -77.70550467234690473, 36.35194583547913538 ) ) ;
#12251 = AXIS2_PLACEMENT_3D ( 'NONE', #4928, #19134, #17505 ) ;
#12252 = CARTESIAN_POINT ( 'NONE',  ( -4.581103194069770623, 3.453261854572849288, 293.5832628385307999 ) ) ;
#12253 = VERTEX_POINT ( 'NONE', #4371 ) ;
#12254 = CARTESIAN_POINT ( 'NONE',  ( -50.93469132750304595, -59.42266395395774481, 132.4711112102474146 ) ) ;
#12255 = DIRECTION ( 'NONE',  ( 0.3088643371590125142, -0.9511061040868803440, 0.000000000000000000 ) ) ;
#12256 = EDGE_LOOP ( 'NONE', ( #15399, #19315, #246, #8911 ) ) ;
#12257 = EDGE_CURVE ( 'NONE', #5706, #13158, #9403, .T. ) ;
#12258 = EDGE_CURVE ( 'NONE', #6317, #2094, #6799, .T. ) ;
#12259 = ORIENTED_EDGE ( 'NONE', *, *, #5515, .F. ) ;
#12260 = EDGE_CURVE ( 'NONE', #9227, #9534, #13291, .T. ) ;
#12261 = PRODUCT_DEFINITION ( 'UNKNOWN', '', #3289, #1518 ) ;
#12262 = DIRECTION ( 'NONE',  ( 1.000000000000000000, 0.000000000000000000, 0.000000000000000000 ) ) ;
#12263 = ORIENTED_EDGE ( 'NONE', *, *, #19119, .F. ) ;
#12264 = CIRCLE ( 'NONE', #17194, 7.500000000000020428 ) ;
#12265 = DIRECTION ( 'NONE',  ( -0.9009688679024212554, 0.4338837391175534575, 0.000000000000000000 ) ) ;
#12266 = CARTESIAN_POINT ( 'NONE',  ( -181.0783081749256382, -200.0000000000000284, 40.00000000000000000 ) ) ;
#12267 = EDGE_LOOP ( 'NONE', ( #8957, #3650, #8467, #10294, #13956, #14841, #3398, #17368, #18748, #1453, #2019, #16651, #12315, #15805, #7235, #8062, #596, #16696, #11999, #14951, #413, #2639, #3916, #3989, #14313, #5434, #14991, #17447, #3185, #19472, #11870, #12718, #6607, #5859, #3045, #18873, #8303, #11544, #2511, #9855, #20, #4633, #6372, #12425, #10061, #17077, #17964, #14120, #8447, #15312, #17859, #16073, #1938, #14645, #13652, #19824, #4141, #1556, #8504, #11163, #12924, #2951, #1802, #18142, #19452, #2070, #17260, #19100, #6150, #18448, #5985, #12383, #19753, #802, #16981, #12048, #2463, #1758, #14423, #3647, #13718, #18533, #17529, #18440, #12942, #13555, #4238, #11812, #10513, #17730, #12540, #1528, #12695, #17821, #3020, #8642, #574, #8048, #1211, #12100, #11770, #5851, #11340, #10419, #3400, #8578, #12056, #2399, #8136, #19210, #19986, #1312, #9478, #2451, #12698, #822, #12996, #4280, #15494, #7845, #19203, #16746, #15410, #5123, #4865, #3354, #4984, #5099, #12326, #3918, #11872, #3936, #15654, #1106, #192, #16207, #2407, #9147, #13800, #2608, #10901, #1992, #11136, #16340 ) ) ;
#12268 = AXIS2_PLACEMENT_3D ( 'NONE', #19714, #8869, #16268 ) ;
#12269 = CARTESIAN_POINT ( 'NONE',  ( 97.38440206417672584, -115.5262529913685654, 10.24763045490705693 ) ) ;
#12270 = DIRECTION ( 'NONE',  ( 0.8660254037844363761, 0.5000000000000039968, -0.000000000000000000 ) ) ;
#12271 = ADVANCED_FACE ( 'NONE', ( #15314 ), #1307, .F. ) ;
#12272 = CARTESIAN_POINT ( 'NONE',  ( -2.605298826210324936, -5.111158570922258448, 293.5832628385307999 ) ) ;
#12273 = FACE_BOUND ( 'NONE', #10371, .T. ) ;
#12274 = DIRECTION ( 'NONE',  ( 6.982962677686266711E-15, -0.000000000000000000, 1.000000000000000000 ) ) ;
#12275 = CARTESIAN_POINT ( 'NONE',  ( 0.000000000000000000, 0.000000000000000000, 293.5832628385307999 ) ) ;
#12276 = FACE_OUTER_BOUND ( 'NONE', #13869, .T. ) ;
#12277 = CARTESIAN_POINT ( 'NONE',  ( 83.29234334534426409, -124.7495837542613799, 37.24802726318616664 ) ) ;
#12278 = AXIS2_PLACEMENT_3D ( 'NONE', #6288, #8380, #3312 ) ;
#12279 = EDGE_LOOP ( 'NONE', ( #15599, #3294, #16871, #15352, #3497, #13230 ) ) ;
#12280 = FACE_OUTER_BOUND ( 'NONE', #4927, .T. ) ;
#12281 = FACE_OUTER_BOUND ( 'NONE', #5437, .T. ) ;
#12282 = EDGE_CURVE ( 'NONE', #12185, #5313, #10399, .T. ) ;
#12283 = ORIENTED_EDGE ( 'NONE', *, *, #16466, .T. ) ;
#12285 = VERTEX_POINT ( 'NONE', #16657 ) ;
#12284 = VECTOR ( 'NONE', #16254, 1000.000000000000000 ) ;
#12286 = ORIENTED_EDGE ( 'NONE', *, *, #4921, .F. ) ;
#12287 = ADVANCED_FACE ( 'NONE', ( #15109 ), #1089, .F. ) ;
#12288 = CARTESIAN_POINT ( 'NONE',  ( -181.0783081749256382, -200.0000000000000284, 0.000000000000000000 ) ) ;
#12289 = ORIENTED_EDGE ( 'NONE', *, *, #5, .F. ) ;
#12290 = FACE_OUTER_BOUND ( 'NONE', #1502, .T. ) ;
#12291 = DIRECTION ( 'NONE',  ( 0.000000000000000000, 0.000000000000000000, 1.000000000000000000 ) ) ;
#12292 = CARTESIAN_POINT ( 'NONE',  ( -15.91767397667354800, 141.9028892025177413, 39.99999999999999289 ) ) ;
#12293 = AXIS2_PLACEMENT_3D ( 'NONE', #11739, #13571, #7343 ) ;
#12294 = CIRCLE ( 'NONE', #1177, 9.000000000000000000 ) ;
#12295 = CARTESIAN_POINT ( 'NONE',  ( -57.94128254008190027, -9.381844291199545438, 248.9926560891072143 ) ) ;
#12296 = LINE ( 'NONE', #19669, #2568 ) ;
#12297 = LINE ( 'NONE', #12084, #12403 ) ;
#12298 = FACE_OUTER_BOUND ( 'NONE', #318, .T. ) ;
#12299 = CARTESIAN_POINT ( 'NONE',  ( -134.6268015237251632, -73.65543454550571312, 7.414222461414868626 ) ) ;
#12300 = CARTESIAN_POINT ( 'NONE',  ( 133.5474595738625680, -68.30173510457201758, -0.05649235984010308326 ) ) ;
#12301 = PLANE ( 'NONE',  #9836 ) ;
#12302 = CARTESIAN_POINT ( 'NONE',  ( -127.0298602564943735, -79.77387071030869947, 48.90123617796809441 ) ) ;
#12303 = VERTEX_POINT ( 'NONE', #4268 ) ;
#12304 = DIRECTION ( 'NONE',  ( 1.000000000000000000, 0.000000000000000000, 0.000000000000000000 ) ) ;
#12305 = ORIENTED_EDGE ( 'NONE', *, *, #8414, .F. ) ;
#12306 = ORIENTED_EDGE ( 'NONE', *, *, #13672, .F. ) ;
#12307 = VECTOR ( 'NONE', #12454, 1000.000000000000000 ) ;
#12308 = ORIENTED_EDGE ( 'NONE', *, *, #7386, .F. ) ;
#12309 = CARTESIAN_POINT ( 'NONE',  ( -144.1596479796006349, -15.14334797026772783, -2.639547494419652196 ) ) ;
#12310 = CARTESIAN_POINT ( 'NONE',  ( 0.000000000000000000, 0.000000000000000000, -105.0000000000000142 ) ) ;
#12311 = FACE_OUTER_BOUND ( 'NONE', #3960, .T. ) ;
#12312 = ORIENTED_EDGE ( 'NONE', *, *, #4109, .T. ) ;
#12313 = DIRECTION ( 'NONE',  ( -0.000000000000000000, -0.000000000000000000, -1.000000000000000000 ) ) ;
#12314 = LINE ( 'NONE', #18686, #647 ) ;
#12315 = ORIENTED_EDGE ( 'NONE', *, *, #12515, .T. ) ;
#12316 = DIRECTION ( 'NONE',  ( 0.000000000000000000, 0.000000000000000000, 1.000000000000000000 ) ) ;
#12317 = DIRECTION ( 'NONE',  ( 1.000000000000000000, 0.000000000000000000, -6.976128451377902853E-15 ) ) ;
#12318 = DIRECTION ( 'NONE',  ( -1.000000000000000000, 0.000000000000000000, 0.000000000000000000 ) ) ;
#12319 = CARTESIAN_POINT ( 'NONE',  ( 25.47058595421554372, 74.01264520835162841, 248.9926560891072143 ) ) ;
#12320 = PLANE ( 'NONE',  #2653 ) ;
#12321 = AXIS2_PLACEMENT_3D ( 'NONE', #6925, #19209, #2223 ) ;
#12322 = AXIS2_PLACEMENT_3D ( 'NONE', #12838, #14948, #7189 ) ;
#12323 = VECTOR ( 'NONE', #5469, 1000.000000000000000 ) ;
#12324 = DIRECTION ( 'NONE',  ( -0.8660254037844432595, 0.4999999999999919509, 0.000000000000000000 ) ) ;
#12325 = CARTESIAN_POINT ( 'NONE',  ( -5.951998377315478983, -25.21111933077039069, 39.88498244535549730 ) ) ;
#12326 = ORIENTED_EDGE ( 'NONE', *, *, #13024, .T. ) ;
#12327 = VERTEX_POINT ( 'NONE', #10496 ) ;
#12328 = ORIENTED_EDGE ( 'NONE', *, *, #17392, .T. ) ;
#12329 = ORIENTED_EDGE ( 'NONE', *, *, #12973, .F. ) ;
#12330 = ADVANCED_FACE ( 'NONE', ( #2744 ), #8965, .F. ) ;
#12331 = DIRECTION ( 'NONE',  ( -6.982962677686266711E-15, 1.972152263052529076E-31, -1.000000000000000000 ) ) ;
#12332 = ORIENTED_EDGE ( 'NONE', *, *, #19518, .T. ) ;
#12333 = LINE ( 'NONE', #4576, #16546 ) ;
#12334 = AXIS2_PLACEMENT_3D ( 'NONE', #15809, #1793, #16112 ) ;
#12335 = CARTESIAN_POINT ( 'NONE',  ( -28.15057869795625578, -51.51682027493055216, 132.4711112102474146 ) ) ;
#12336 = VECTOR ( 'NONE', #4489, 1000.000000000000000 ) ;
#12337 = SURFACE_STYLE_FILL_AREA ( #1192 ) ;
#12338 = CARTESIAN_POINT ( 'NONE',  ( -50.41613078340781584, 30.05702882063080494, 248.9926560891072143 ) ) ;
#12339 = ORIENTED_EDGE ( 'NONE', *, *, #2499, .T. ) ;
#12340 = EDGE_CURVE ( 'NONE', #15515, #4038, #17172, .T. ) ;
#12341 = CARTESIAN_POINT ( 'NONE',  ( 0.3570196857253458145, 6.047589086024989236, -7.525268439705685708 ) ) ;
#12342 = CARTESIAN_POINT ( 'NONE',  ( 57.92514141135453087, 18.28503710798568349, 293.5832628385307999 ) ) ;
#12343 = ORIENTED_EDGE ( 'NONE', *, *, #13761, .T. ) ;
#12344 = EDGE_CURVE ( 'NONE', #13855, #4859, #8248, .T. ) ;
#12345 = UNCERTAINTY_MEASURE_WITH_UNIT (LENGTH_MEASURE( 1.000000000000000082E-05 ), #19961, 'distance_accuracy_value', 'NONE');
#12346 = FACE_BOUND ( 'NONE', #10758, .T. ) ;
#12347 = DIRECTION ( 'NONE',  ( 0.000000000000000000, 0.000000000000000000, 1.000000000000000000 ) ) ;
#12348 = EDGE_CURVE ( 'NONE', #7939, #14390, #2538, .T. ) ;
#12349 = EDGE_CURVE ( 'NONE', #17792, #13097, #1816, .T. ) ;
#12350 = DIRECTION ( 'NONE',  ( 1.000000000000000000, 0.000000000000000000, 0.000000000000000000 ) ) ;
#12351 = AXIS2_PLACEMENT_3D ( 'NONE', #13070, #16264, #9912 ) ;
#12352 = DIRECTION ( 'NONE',  ( -0.5300553768524346454, -0.8479630283625717579, 0.000000000000000000 ) ) ;
#12353 = CARTESIAN_POINT ( 'NONE',  ( -134.7088403748421399, -73.01573503433813528, 30.97892361658604443 ) ) ;
#12354 = CARTESIAN_POINT ( 'NONE',  ( -107.3244020400115062, 89.90100472445219282, 39.90192053207060496 ) ) ;
#12355 = AXIS2_PLACEMENT_3D ( 'NONE', #12082, #5969, #7491 ) ;
#12356 = AXIS2_PLACEMENT_3D ( 'NONE', #5818, #4071, #7247 ) ;
#12357 = ORIENTED_EDGE ( 'NONE', *, *, #8872, .F. ) ;
#12358 = CIRCLE ( 'NONE', #18232, 15.91767397667354089 ) ;
#12359 = PLANE ( 'NONE',  #16600 ) ;
#12360 = DIRECTION ( 'NONE',  ( -0.000000000000000000, -0.000000000000000000, -1.000000000000000000 ) ) ;
#12361 = ORIENTED_EDGE ( 'NONE', *, *, #11268, .F. ) ;
#12362 = VERTEX_POINT ( 'NONE', #18705 ) ;
#12363 = EDGE_CURVE ( 'NONE', #12139, #10138, #3556, .T. ) ;
#12364 = CARTESIAN_POINT ( 'NONE',  ( 22.29928840491073672, 56.50138340076680521, 283.5832628385307999 ) ) ;
#12365 = ORIENTED_EDGE ( 'NONE', *, *, #13031, .T. ) ;
#12366 = CARTESIAN_POINT ( 'NONE',  ( 47.56406379474552182, 37.78325588002191893, 283.5832628385307999 ) ) ;
#12367 = DIRECTION ( 'NONE',  ( 1.000000000000000000, 0.000000000000000000, -0.000000000000000000 ) ) ;
#12368 = ORIENTED_EDGE ( 'NONE', *, *, #1942, .T. ) ;
#12369 = CARTESIAN_POINT ( 'NONE',  ( 96.12355554546724079, -116.0165654454190047, 9.818202592590962396 ) ) ;
#12370 = CARTESIAN_POINT ( 'NONE',  ( -8.402595070145098433, -117.5408478153264298, 14.88498244535551152 ) ) ;
#12371 = AXIS2_PLACEMENT_3D ( 'NONE', #12015, #1289, #9051 ) ;
#12372 = AXIS2_PLACEMENT_3D ( 'NONE', #9495, #17068, #18708 ) ;
#12373 = VECTOR ( 'NONE', #4149, 1000.000000000000000 ) ;
#12374 = EDGE_CURVE ( 'NONE', #1323, #5389, #18215, .T. ) ;
#12375 = EDGE_CURVE ( 'NONE', #15549, #16453, #17377, .T. ) ;
#12376 = CARTESIAN_POINT ( 'NONE',  ( -140.7803916714547086, -18.74395295176650578, -17.77646390483898386 ) ) ;
#12377 = DIRECTION ( 'NONE',  ( 0.000000000000000000, 0.000000000000000000, -1.000000000000000000 ) ) ;
#12378 = EDGE_LOOP ( 'NONE', ( #5605, #14613, #18410, #18538 ) ) ;
#12379 = FACE_OUTER_BOUND ( 'NONE', #2138, .T. ) ;
#12380 = CARTESIAN_POINT ( 'NONE',  ( 118.3534152657848608, 114.7431683447366595, 60.00000000000000000 ) ) ;
#12381 = FACE_OUTER_BOUND ( 'NONE', #9933, .T. ) ;
#12382 = CARTESIAN_POINT ( 'NONE',  ( 96.05955731895404881, -115.3262050113700496, 35.20779912320998761 ) ) ;
#12383 = ORIENTED_EDGE ( 'NONE', *, *, #8974, .T. ) ;
#12384 = CYLINDRICAL_SURFACE ( 'NONE', #11998, 3.224098631618460331 ) ;
#12385 = PLANE ( 'NONE',  #6319 ) ;
#12386 = ORIENTED_EDGE ( 'NONE', *, *, #11017, .F. ) ;
#12387 = AXIS2_PLACEMENT_3D ( 'NONE', #11095, #7826, #17358 ) ;
#12388 = AXIS2_PLACEMENT_3D ( 'NONE', #18886, #12424, #14066 ) ;
#12389 = ORIENTED_EDGE ( 'NONE', *, *, #12375, .F. ) ;
#12390 = EDGE_CURVE ( 'NONE', #7405, #9578, #16586, .T. ) ;
#12391 = DIRECTION ( 'NONE',  ( 0.000000000000000000, -1.000000000000000000, 0.000000000000000000 ) ) ;
#12392 = VERTEX_POINT ( 'NONE', #76 ) ;
#12393 = CARTESIAN_POINT ( 'NONE',  ( -103.6585128263304938, -125.0478522927852794, 0.7634766421525948088 ) ) ;
#12394 = FACE_OUTER_BOUND ( 'NONE', #537, .T. ) ;
#12395 = VERTEX_POINT ( 'NONE', #17275 ) ;
#12396 = DIRECTION ( 'NONE',  ( 0.6234898018587442525, -0.7818314824680211439, 0.000000000000000000 ) ) ;
#12397 = DIRECTION ( 'NONE',  ( -0.1390141521205912334, 0.9902903945359629034, 0.000000000000000000 ) ) ;
#12398 = CARTESIAN_POINT ( 'NONE',  ( 132.4160198941376620, -70.47193775266622140, 42.82081320361049137 ) ) ;
#12399 = CARTESIAN_POINT ( 'NONE',  ( -93.44030642264235098, -117.3428525121095447, 48.41348831998372049 ) ) ;
#12400 = EDGE_CURVE ( 'NONE', #11659, #2362, #18547, .T. ) ;
#12401 = DIRECTION ( 'NONE',  ( -0.000000000000000000, -0.000000000000000000, 1.000000000000000000 ) ) ;
#12402 = CARTESIAN_POINT ( 'NONE',  ( 59.06449708980161972, 51.36153797460926995, 248.9926560891072143 ) ) ;
#12403 = VECTOR ( 'NONE', #6184, 999.9999999999998863 ) ;
#12404 = ADVANCED_FACE ( 'NONE', ( #19015 ), #3153, .T. ) ;
#12405 = CARTESIAN_POINT ( 'NONE',  ( 0.000000000000000000, 0.000000000000000000, 283.5832628385307999 ) ) ;
#12406 = CARTESIAN_POINT ( 'NONE',  ( -134.7188131032333445, -72.93593548660992099, 10.00000000000000533 ) ) ;
#12407 = CARTESIAN_POINT ( 'NONE',  ( 123.8565975624208733, -84.62454961665271469, -0.6152758568786554916 ) ) ;
#12408 = DIRECTION ( 'NONE',  ( -1.000000000000000000, 0.000000000000000000, 7.137148015447434001E-15 ) ) ;
#12409 = FACE_OUTER_BOUND ( 'NONE', #147, .T. ) ;
#12410 = CARTESIAN_POINT ( 'NONE',  ( -132.5080654097351953, -70.41765848030097175, 35.03383174997027538 ) ) ;
#12411 = EDGE_CURVE ( 'NONE', #6110, #244, #17580, .T. ) ;
#12412 = ORIENTED_EDGE ( 'NONE', *, *, #18916, .T. ) ;
#12413 = CARTESIAN_POINT ( 'NONE',  ( 156.4179374840099683, -52.02840013023883614, 49.99999999999999289 ) ) ;
#12414 = ADVANCED_FACE ( 'NONE', ( #14089 ), #4996, .T. ) ;
#12415 = VECTOR ( 'NONE', #4806, 1000.000000000000000 ) ;
#12416 = VERTEX_POINT ( 'NONE', #15730 ) ;
#12417 = AXIS2_PLACEMENT_3D ( 'NONE', #12405, #18665, #4641 ) ;
#12418 = ORIENTED_EDGE ( 'NONE', *, *, #4734, .F. ) ;
#12419 = ORIENTED_EDGE ( 'NONE', *, *, #6854, .F. ) ;
#12420 = DIRECTION ( 'NONE',  ( -0.000000000000000000, -0.000000000000000000, 1.000000000000000000 ) ) ;
#12421 = DIRECTION ( 'NONE',  ( -0.000000000000000000, -0.000000000000000000, 1.000000000000000000 ) ) ;
#12422 = ORIENTED_EDGE ( 'NONE', *, *, #14367, .F. ) ;
#12423 = DIRECTION ( 'NONE',  ( 1.000000000000000000, 0.000000000000000000, 0.000000000000000000 ) ) ;
#12424 = DIRECTION ( 'NONE',  ( 0.000000000000000000, 0.000000000000000000, -1.000000000000000000 ) ) ;
#12425 = ORIENTED_EDGE ( 'NONE', *, *, #1243, .T. ) ;
#12426 = CARTESIAN_POINT ( 'NONE',  ( -107.2897435581724608, 77.67224767425115317, -29.92169227468260573 ) ) ;
#12427 = DIRECTION ( 'NONE',  ( 6.982962677686266711E-15, -0.000000000000000000, 1.000000000000000000 ) ) ;
#12428 = CARTESIAN_POINT ( 'NONE',  ( -110.0000000000000000, 275.0000000000000000, 104.9999999999999858 ) ) ;
#12429 = DIRECTION ( 'NONE',  ( 0.3420201433256790380, -0.9396926207859046531, 0.000000000000000000 ) ) ;
#12430 = VECTOR ( 'NONE', #9268, 1000.000000000000227 ) ;
#12431 = CARTESIAN_POINT ( 'NONE',  ( 20.21777810286676313, 59.58067424803633827, 248.9926560891072143 ) ) ;
#12432 = CARTESIAN_POINT ( 'NONE',  ( 133.8517991834422105, -78.87665408946898538, 36.99948406166920023 ) ) ;
#12433 = DIRECTION ( 'NONE',  ( 0.000000000000000000, 0.000000000000000000, 1.000000000000000000 ) ) ;
#12434 = EDGE_LOOP ( 'NONE', ( #5502, #7849, #3736 ) ) ;
#12435 = ORIENTED_EDGE ( 'NONE', *, *, #3621, .T. ) ;
#12436 = ORIENTED_EDGE ( 'NONE', *, *, #10120, .F. ) ;
#12437 = ORIENTED_EDGE ( 'NONE', *, *, #13465, .T. ) ;
#12438 = CARTESIAN_POINT ( 'NONE',  ( 0.000000000000000000, 0.000000000000000000, 293.5832628385307999 ) ) ;
#12439 = AXIS2_PLACEMENT_3D ( 'NONE', #15090, #16544, #19602 ) ;
#12440 = EDGE_LOOP ( 'NONE', ( #10659, #16467, #19278, #11934, #4443, #18729, #13607, #10426, #7607, #11294, #17721, #674, #3499, #9119, #10725, #17818 ) ) ;
#12441 = CARTESIAN_POINT ( 'NONE',  ( -1.629937663769596368, -60.72279549541552512, 293.5832628385307999 ) ) ;
#12442 = VECTOR ( 'NONE', #7809, 1000.000000000000000 ) ;
#12443 = CARTESIAN_POINT ( 'NONE',  ( 73.82206860051529418, 25.99419088092216867, 248.9926560891072143 ) ) ;
#12444 = CARTESIAN_POINT ( 'NONE',  ( -52.50000000000000000, -2.094888803305880013E-13, -105.0000000000000142 ) ) ;
#12445 = DIRECTION ( 'NONE',  ( -0.000000000000000000, -0.000000000000000000, 1.000000000000000000 ) ) ;
#12446 = ORIENTED_EDGE ( 'NONE', *, *, #13211, .T. ) ;
#12447 = PLANE ( 'NONE',  #4739 ) ;
#12448 = DIRECTION ( 'NONE',  ( -0.000000000000000000, -0.000000000000000000, 1.000000000000000000 ) ) ;
#12449 = ORIENTED_EDGE ( 'NONE', *, *, #10163, .T. ) ;
#12450 = CARTESIAN_POINT ( 'NONE',  ( -73.42392789539788112, 130.8023724896636679, -11.24819646464914413 ) ) ;
#12451 = CARTESIAN_POINT ( 'NONE',  ( 4.189777606611760026E-13, -60.00000000000000000, -115.0000000000000000 ) ) ;
#12452 = ADVANCED_FACE ( 'NONE', ( #7844 ), #12755, .T. ) ;
#12453 = CARTESIAN_POINT ( 'NONE',  ( 176.1792632384392334, -186.5724904703758682, 10.00000000000000178 ) ) ;
#12454 = DIRECTION ( 'NONE',  ( -0.9396926207859046531, -0.3420201433256790380, -0.000000000000000000 ) ) ;
#12455 = CARTESIAN_POINT ( 'NONE',  ( 39.80940113486020238, -48.72193424476462553, 293.5832628385307999 ) ) ;
#12456 = CARTESIAN_POINT ( 'NONE',  ( -94.22720848804412697, 103.5554077689919410, 36.27354526481243369 ) ) ;
#12457 = ORIENTED_EDGE ( 'NONE', *, *, #19387, .F. ) ;
#12458 = CARTESIAN_POINT ( 'NONE',  ( 159.9599531637113330, -36.50981547336952104, 60.00000000000000000 ) ) ;
#12459 = VERTEX_POINT ( 'NONE', #4689 ) ;
#12460 = VERTEX_POINT ( 'NONE', #11216 ) ;
#12461 = CARTESIAN_POINT ( 'NONE',  ( -63.68887634719365565, -147.8252249328922687, 49.99999999999999289 ) ) ;
#12462 = EDGE_CURVE ( 'NONE', #141, #12565, #6329, .T. ) ;
#12463 = EDGE_LOOP ( 'NONE', ( #4548, #11002, #13847, #1833, #3472, #19680, #11416, #14315, #2796, #4037, #716, #6467, #6768, #14859, #4375, #1370, #5485, #991, #18265, #20222, #14584, #12179, #5702, #917, #18367, #8425, #7747, #15857, #3691, #14199, #19036, #2622, #6800, #10643, #6321, #6422, #3287, #13562, #13080, #1473, #8078, #1207, #16557, #10364, #7988, #2148, #18037, #10606, #434, #16255, #13288, #14244, #2144, #6393, #17990, #9192, #6294, #1171, #2610, #17545, #19495, #9066, #13047, #16628, #19807, #12596, #7027, #8862, #16904, #4985, #15602, #16233, #4012, #8315, #6896, #268, #9169, #6169, #2120, #1649, #396, #6941, #12457, #17742, #1137, #2686, #4837, #18333, #1183, #8271, #16698, #10576, #8687, #7788, #13440, #12723, #3696, #6866, #19954, #13386, #17069, #13464, #4500, #17829, #4074, #16216, #9461, #7373, #6424, #12286, #8887, #18356, #19397, #18749, #6796, #591, #468, #7817, #623, #10809, #7991, #15812, #9635, #10555, #1090, #2882, #12041, #18175, #3076, #10119, #8544, #2564, #8954, #6578, #210, #1481, #8792, #11569, #17674, #1350, #1912, #13489, #5781, #19963 ) ) ;
#12464 = EDGE_CURVE ( 'NONE', #18654, #17774, #17479, .T. ) ;
#12465 = DIRECTION ( 'NONE',  ( -0.000000000000000000, -0.000000000000000000, 1.000000000000000000 ) ) ;
#12466 = PLANE ( 'NONE',  #17761 ) ;
#12467 = EDGE_LOOP ( 'NONE', ( #9400, #7718 ) ) ;
#12468 = DIRECTION ( 'NONE',  ( -0.9271237148521547233, 0.3747554100459928872, 0.000000000000000000 ) ) ;
#12469 = CARTESIAN_POINT ( 'NONE',  ( -10.11498556985118746, 62.09913334491134407, 132.4711112102474146 ) ) ;
#12470 = VECTOR ( 'NONE', #9646, 1000.000000000000000 ) ;
#12471 = ADVANCED_FACE ( 'NONE', ( #7946 ), #15835, .F. ) ;
#12472 = DIRECTION ( 'NONE',  ( 0.6155349844899715706, -0.7881095627315598540, 0.000000000000000000 ) ) ;
#12473 = DIRECTION ( 'NONE',  ( -0.3420201433256790380, 0.9396926207859046531, 0.000000000000000000 ) ) ;
#12474 = VERTEX_POINT ( 'NONE', #8152 ) ;
#12475 = DIRECTION ( 'NONE',  ( -0.000000000000000000, -0.000000000000000000, 1.000000000000000000 ) ) ;
#12476 = FACE_OUTER_BOUND ( 'NONE', #11429, .T. ) ;
#12477 = CARTESIAN_POINT ( 'NONE',  ( 60.83768308848377160, -49.24833719034207036, 110.7293897666001214 ) ) ;
#12478 = CARTESIAN_POINT ( 'NONE',  ( 95.50801338652755135, -116.1654322105723480, 31.50148117855486518 ) ) ;
#12479 = ORIENTED_EDGE ( 'NONE', *, *, #8530, .F. ) ;
#12480 = PLANE ( 'NONE',  #1567 ) ;
#12481 = CARTESIAN_POINT ( 'NONE',  ( -49.24833719034228352, -60.83768308848358686, 132.4711112102474146 ) ) ;
#12482 = VERTEX_POINT ( 'NONE', #13340 ) ;
#12483 = ORIENTED_EDGE ( 'NONE', *, *, #17244, .T. ) ;
#12484 = ORIENTED_EDGE ( 'NONE', *, *, #4894, .F. ) ;
#12485 = EDGE_CURVE ( 'NONE', #12798, #6114, #891, .T. ) ;
#12486 = AXIS2_PLACEMENT_3D ( 'NONE', #17448, #9653, #3421 ) ;
#12487 = CIRCLE ( 'NONE', #14462, 150.0000000000000284 ) ;
#12488 = EDGE_CURVE ( 'NONE', #20112, #7117, #16536, .T. ) ;
#12489 = ORIENTED_EDGE ( 'NONE', *, *, #4686, .T. ) ;
#12490 = EDGE_CURVE ( 'NONE', #4348, #9722, #4830, .T. ) ;
#12491 = CARTESIAN_POINT ( 'NONE',  ( -105.6220017318342315, -121.8343408522481468, 0.1250734579962385629 ) ) ;
#12492 = FACE_BOUND ( 'NONE', #1895, .T. ) ;
#12493 = ORIENTED_EDGE ( 'NONE', *, *, #1880, .F. ) ;
#12494 = VECTOR ( 'NONE', #7447, 1000.000000000000000 ) ;
#12495 = LINE ( 'NONE', #9123, #5025 ) ;
#12496 = DIRECTION ( 'NONE',  ( 0.000000000000000000, 1.000000000000000000, 0.000000000000000000 ) ) ;
#12497 = DIRECTION ( 'NONE',  ( 0.000000000000000000, 0.000000000000000000, 1.000000000000000000 ) ) ;
#12498 = CARTESIAN_POINT ( 'NONE',  ( -100.3336596192664416, -130.0766330734951453, 36.97651187266671258 ) ) ;
#12499 = CARTESIAN_POINT ( 'NONE',  ( 7.350000000000000533, -5.196152422706607155, 8.999999999999998224 ) ) ;
#12500 = CYLINDRICAL_SURFACE ( 'NONE', #8820, 42.50000000000000000 ) ;
#12501 = EDGE_CURVE ( 'NONE', #7604, #2094, #19406, .T. ) ;
#12502 = CARTESIAN_POINT ( 'NONE',  ( 71.18887634719571622, -147.8252249328912740, 39.99999999999999289 ) ) ;
#12503 = VECTOR ( 'NONE', #836, 1000.000000000000000 ) ;
#12504 = AXIS2_PLACEMENT_3D ( 'NONE', #377, #14494, #12851 ) ;
#12505 = DIRECTION ( 'NONE',  ( -1.000000000000000000, 0.000000000000000000, 0.000000000000000000 ) ) ;
#12506 = CYLINDRICAL_SURFACE ( 'NONE', #15598, 60.74260934110282051 ) ;
#12507 = CARTESIAN_POINT ( 'NONE',  ( -128.0993248974477581, -78.05374007935974134, 48.25206861699041383 ) ) ;
#12508 = ORIENTED_EDGE ( 'NONE', *, *, #13994, .F. ) ;
#12509 = DIRECTION ( 'NONE',  ( -1.000000000000000000, 0.000000000000000000, 0.000000000000000000 ) ) ;
#12510 = AXIS2_PLACEMENT_3D ( 'NONE', #17369, #6222, #18699 ) ;
#12511 = AXIS2_PLACEMENT_3D ( 'NONE', #17086, #1435, #10936 ) ;
#12512 = ORIENTED_EDGE ( 'NONE', *, *, #16281, .T. ) ;
#12513 = ADVANCED_FACE ( 'NONE', ( #968 ), #11520, .T. ) ;
#12514 = ORIENTED_EDGE ( 'NONE', *, *, #7240, .T. ) ;
#12515 = EDGE_CURVE ( 'NONE', #17279, #14612, #2322, .T. ) ;
#12516 = EDGE_CURVE ( 'NONE', #8307, #13307, #11381, .T. ) ;
#12517 =( BOUNDED_CURVE ( )  B_SPLINE_CURVE ( 3, ( #4233, #19879, #13530, #15275 ),
 .UNSPECIFIED., .F., .F. ) 
 B_SPLINE_CURVE_WITH_KNOTS ( ( 4, 4 ),
 ( 1.570796326794896780, 3.141592653589793116 ),
 .UNSPECIFIED. ) 
 CURVE ( )  GEOMETRIC_REPRESENTATION_ITEM ( )  RATIONAL_B_SPLINE_CURVE ( ( 1.000000000000000000, 0.8047378541243650485, 0.8047378541243650485, 1.000000000000000000 ) ) 
 REPRESENTATION_ITEM ( '' )  );
#12518 = B_SPLINE_CURVE_WITH_KNOTS ( 'NONE', 3,
 ( #4448, #1489, #3028, #10679, #12008, #18467, #13752, #15503, #5791, #12216, #6097, #16831 ),
 .UNSPECIFIED., .F., .F.,
 ( 4, 2, 2, 2, 2, 4 ),
 ( 0.1419734016336355320, 0.1501012059599697024, 0.1582290102863038450, 0.1622929124494709163, 0.1663568146126380154, 0.1744846189389721580 ),
 .UNSPECIFIED. ) ;
#12519 = AXIS2_PLACEMENT_3D ( 'NONE', #12047, #4287, #10512 ) ;
#12520 = ORIENTED_EDGE ( 'NONE', *, *, #8748, .F. ) ;
#12521 = FACE_OUTER_BOUND ( 'NONE', #6762, .T. ) ;
#12522 = DIRECTION ( 'NONE',  ( 0.7818314824680222541, 0.6234898018587428092, 0.000000000000000000 ) ) ;
#12523 = AXIS2_PLACEMENT_3D ( 'NONE', #13433, #5888, #1279 ) ;
#12524 = FACE_OUTER_BOUND ( 'NONE', #3669, .T. ) ;
#12525 = ADVANCED_FACE ( 'NONE', ( #5581 ), #10279, .F. ) ;
#12526 = LINE ( 'NONE', #18786, #2913 ) ;
#12527 = CARTESIAN_POINT ( 'NONE',  ( 71.65703592476599226, -89.51573765728305432, 14.88498244535495196 ) ) ;
#12528 = CARTESIAN_POINT ( 'NONE',  ( 0.000000000000000000, 0.000000000000000000, 283.5832628385307999 ) ) ;
#12529 = COLOUR_RGB ( '', 0.66274510, 0.83137255, 0.94901961) ;
#12530 = LINE ( 'NONE', #5615, #12430 ) ;
#12531 = LINE ( 'NONE', #9473, #15381 ) ;
#12532 = ORIENTED_EDGE ( 'NONE', *, *, #2845, .T. ) ;
#12533 = CARTESIAN_POINT ( 'NONE',  ( 132.8916714744556771, -69.69402298600660117, 33.62506225554120221 ) ) ;
#12534 = CARTESIAN_POINT ( 'NONE',  ( 0.000000000000000000, 0.000000000000000000, 283.5832628385307999 ) ) ;
#12535 = VERTEX_POINT ( 'NONE', #11800 ) ;
#12536 = ORIENTED_EDGE ( 'NONE', *, *, #15149, .F. ) ;
#12537 = VERTEX_POINT ( 'NONE', #18066 ) ;
#12538 = ADVANCED_FACE ( 'NONE', ( #7022 ), #8452, .F. ) ;
#12539 = AXIS2_PLACEMENT_3D ( 'NONE', #15989, #2182, #17635 ) ;
#12540 = ORIENTED_EDGE ( 'NONE', *, *, #5515, .T. ) ;
#12541 = DIRECTION ( 'NONE',  ( 0.5000000000000009992, -0.8660254037844380415, 0.000000000000000000 ) ) ;
#12542 = VECTOR ( 'NONE', #3124, 1000.000000000000000 ) ;
#12543 = ORIENTED_EDGE ( 'NONE', *, *, #6119, .T. ) ;
#12544 = DIRECTION ( 'NONE',  ( -0.3420201433256568335, -0.9396926207859127578, 0.000000000000000000 ) ) ;
#12545 = EDGE_CURVE ( 'NONE', #17498, #16184, #10374, .T. ) ;
#12546 = CARTESIAN_POINT ( 'NONE',  ( -97.83396368271628774, -133.5156904852161404, 32.57277006560284605 ) ) ;
#12547 = CARTESIAN_POINT ( 'NONE',  ( 92.34802049131702972, -66.64338626758360817, 39.88498244535480808 ) ) ;
#12548 = LINE ( 'NONE', #6532, #3080 ) ;
#12549 = DIRECTION ( 'NONE',  ( 0.000000000000000000, 0.000000000000000000, -1.000000000000000000 ) ) ;
#12550 = ORIENTED_EDGE ( 'NONE', *, *, #3897, .F. ) ;
#12551 = CARTESIAN_POINT ( 'NONE',  ( 166.7850001792985495, -199.9999999999999716, 40.00000000000000000 ) ) ;
#12552 = CARTESIAN_POINT ( 'NONE',  ( 0.5584673446549148768, 5.621163452808795036, 8.263859302085863945 ) ) ;
#12553 = ORIENTED_EDGE ( 'NONE', *, *, #4222, .F. ) ;
#12554 = CARTESIAN_POINT ( 'NONE',  ( -84.56545567830508503, 119.8977594044767159, -25.88840230773694628 ) ) ;
#12555 = CARTESIAN_POINT ( 'NONE',  ( -152.4599531637108498, -36.50981547337168109, 49.99999999999999289 ) ) ;
#12556 = CIRCLE ( 'NONE', #16166, 140.0000000000000000 ) ;
#12557 = FACE_OUTER_BOUND ( 'NONE', #11320, .T. ) ;
#12558 = DIRECTION ( 'NONE',  ( -0.9394263059140721683, -0.3427509529624100937, 0.000000000000000000 ) ) ;
#12559 = LINE ( 'NONE', #18823, #12415 ) ;
#12560 = CARTESIAN_POINT ( 'NONE',  ( -84.10089422706629136, 111.9261769101578352, 28.55442653938981579 ) ) ;
#12561 = ORIENTED_EDGE ( 'NONE', *, *, #18529, .T. ) ;
#12562 = DIRECTION ( 'NONE',  ( 0.9396926207859127578, -0.3420201433256568335, 0.000000000000000000 ) ) ;
#12563 = ORIENTED_EDGE ( 'NONE', *, *, #6806, .F. ) ;
#12564 = CIRCLE ( 'NONE', #19789, 3.224098631618461219 ) ;
#12565 = VERTEX_POINT ( 'NONE', #5294 ) ;
#12566 = CARTESIAN_POINT ( 'NONE',  ( -61.81362617575094021, 11.73417718768112294, 293.5832628385307999 ) ) ;
#12567 = VECTOR ( 'NONE', #17072, 1000.000000000000114 ) ;
#12568 = ORIENTED_EDGE ( 'NONE', *, *, #8660, .F. ) ;
#12569 = CARTESIAN_POINT ( 'NONE',  ( -0.8220851292435327196, -58.69016442926522359, 248.9926560891072143 ) ) ;
#12570 = CARTESIAN_POINT ( 'NONE',  ( 0.000000000000000000, 0.000000000000000000, 248.9926560891072143 ) ) ;
#12571 = ORIENTED_EDGE ( 'NONE', *, *, #7489, .F. ) ;
#12572 = CARTESIAN_POINT ( 'NONE',  ( 97.26553299953100407, -115.5756973141527197, 10.32009213879923060 ) ) ;
#12573 = DIRECTION ( 'NONE',  ( 1.000000000000000000, 0.000000000000000000, 0.000000000000000000 ) ) ;
#12574 = PRODUCT_DEFINITION_SHAPE ( 'NONE', 'NONE',  #20243 ) ;
#12575 = CIRCLE ( 'NONE', #8980, 150.0000000000000284 ) ;
#12576 = PLANE ( 'NONE',  #15704 ) ;
#12577 = LINE ( 'NONE', #18840, #18446 ) ;
#12578 = ORIENTED_EDGE ( 'NONE', *, *, #12976, .F. ) ;
#12579 = CARTESIAN_POINT ( 'NONE',  ( 56.50329132715945235, -22.30005961346246579, 283.5832628385307999 ) ) ;
#12580 = DIRECTION ( 'NONE',  ( 1.000000000000000000, 0.000000000000000000, 0.000000000000000000 ) ) ;
#12581 = DIRECTION ( 'NONE',  ( 0.000000000000000000, 1.000000000000000000, 0.000000000000000000 ) ) ;
#12582 = CARTESIAN_POINT ( 'NONE',  ( 97.05807359152579750, -115.6610107838044286, 29.63931307426926409 ) ) ;
#12583 = VERTEX_POINT ( 'NONE', #14884 ) ;
#12584 = DIRECTION ( 'NONE',  ( 0.4999999999999949485, 0.8660254037844415942, -0.000000000000000000 ) ) ;
#12585 = CARTESIAN_POINT ( 'NONE',  ( -72.90901369577932201, 131.0915673072731806, 20.08013286166580613 ) ) ;
#12586 = ORIENTED_EDGE ( 'NONE', *, *, #15653, .F. ) ;
#12587 = AXIS2_PLACEMENT_3D ( 'NONE', #4642, #10867, #15587 ) ;
#12588 = VERTEX_POINT ( 'NONE', #17773 ) ;
#12589 = VERTEX_POINT ( 'NONE', #4044 ) ;
#12590 = CIRCLE ( 'NONE', #515, 60.74260934110282051 ) ;
#12591 = ORIENTED_EDGE ( 'NONE', *, *, #6786, .F. ) ;
#12592 = ADVANCED_FACE ( 'NONE', ( #8649 ), #11616, .T. ) ;
#12593 = CARTESIAN_POINT ( 'NONE',  ( -97.49999999999998579, -133.9542832461881687, 10.00000000000000178 ) ) ;
#12594 = EDGE_CURVE ( 'NONE', #3496, #6273, #16298, .T. ) ;
#12595 = DIRECTION ( 'NONE',  ( -0.7660444431189792347, 0.6427876096865379196, 0.000000000000000000 ) ) ;
#12596 = ORIENTED_EDGE ( 'NONE', *, *, #1601, .F. ) ;
#12597 = FACE_OUTER_BOUND ( 'NONE', #4269, .T. ) ;
#12598 = FACE_OUTER_BOUND ( 'NONE', #13639, .T. ) ;
#12599 = CARTESIAN_POINT ( 'NONE',  ( -2.240720816136042348, 5.281164089014786178, 283.5832628385307999 ) ) ;
#12600 = CARTESIAN_POINT ( 'NONE',  ( -87.56486837567058501, -121.7886324248894141, 44.19056895215663161 ) ) ;
#12601 = DIRECTION ( 'NONE',  ( 0.000000000000000000, 0.000000000000000000, -1.000000000000000000 ) ) ;
#12602 = AXIS2_PLACEMENT_3D ( 'NONE', #5892, #16935, #5997 ) ;
#12603 = CARTESIAN_POINT ( 'NONE',  ( -93.80830170559219994, -117.0490297264385617, -8.575456544257738400 ) ) ;
#12604 = DIRECTION ( 'NONE',  ( -0.6427876096865300370, -0.7660444431189858960, 0.000000000000000000 ) ) ;
#12605 = EDGE_CURVE ( 'NONE', #12395, #6900, #7125, .T. ) ;
#12606 = CARTESIAN_POINT ( 'NONE',  ( -150.0000000000000284, 0.6141387166827441124, 4.682860153518817015 ) ) ;
#12607 = EDGE_CURVE ( 'NONE', #2991, #11485, #13236, .T. ) ;
#12608 = CYLINDRICAL_SURFACE ( 'NONE', #4610, 15.91767397667354089 ) ;
#12609 = CARTESIAN_POINT ( 'NONE',  ( 42.50000000000000000, 0.000000000000000000, -120.0000000000000142 ) ) ;
#12610 = CARTESIAN_POINT ( 'NONE',  ( -131.5402663983530545, -89.84204999193647723, 39.94380265023705334 ) ) ;
#12611 = VERTEX_POINT ( 'NONE', #5199 ) ;
#12612 = ADVANCED_FACE ( 'NONE', ( #3654 ), #13978, .T. ) ;
#12613 = AXIS2_PLACEMENT_3D ( 'NONE', #4794, #17277, #2026 ) ;
#12614 = CARTESIAN_POINT ( 'NONE',  ( 0.8220851292435327196, 78.26059000578311498, 248.9926560891072143 ) ) ;
#12615 = ORIENTED_EDGE ( 'NONE', *, *, #10383, .F. ) ;
#12616 = AXIS2_PLACEMENT_3D ( 'NONE', #20129, #10711, #15320 ) ;
#12617 = EDGE_LOOP ( 'NONE', ( #4963, #2981, #2858, #8737 ) ) ;
#12618 = ADVANCED_FACE ( 'NONE', ( #3843 ), #17871, .T. ) ;
#12619 = VECTOR ( 'NONE', #2687, 1000.000000000000000 ) ;
#12620 = ORIENTED_EDGE ( 'NONE', *, *, #9158, .F. ) ;
#12621 = CARTESIAN_POINT ( 'NONE',  ( -144.8652878778347599, -14.27854090756834360, 1.773752675255029221 ) ) ;
#12622 = VECTOR ( 'NONE', #4807, 1000.000000000000000 ) ;
#12623 = DIRECTION ( 'NONE',  ( 1.000000000000000000, 0.000000000000000000, 0.000000000000000000 ) ) ;
#12624 = FACE_OUTER_BOUND ( 'NONE', #16208, .T. ) ;
#12625 = CARTESIAN_POINT ( 'NONE',  ( 141.8871031824808995, -16.05777877957299538, 49.99999999999999289 ) ) ;
#12626 = DIRECTION ( 'NONE',  ( -0.000000000000000000, -0.000000000000000000, 1.000000000000000000 ) ) ;
#12627 = DIRECTION ( 'NONE',  ( 0.000000000000000000, 0.000000000000000000, 1.000000000000000000 ) ) ;
#12628 = CARTESIAN_POINT ( 'NONE',  ( 68.46530598706793569, -37.93579148621486041, 248.9926560891072143 ) ) ;
#12629 = CARTESIAN_POINT ( 'NONE',  ( 30.25670013172214468, 55.16472960512381718, 293.5832628385307999 ) ) ;
#12630 = EDGE_CURVE ( 'NONE', #16844, #18605, #8844, .T. ) ;
#12631 = CARTESIAN_POINT ( 'NONE',  ( 107.5000000000000142, -118.5063289449133492, 40.00000000000000000 ) ) ;
#12632 = LINE ( 'NONE', #6613, #15941 ) ;
#12633 = VECTOR ( 'NONE', #18471, 1000.000000000000000 ) ;
#12634 = ADVANCED_FACE ( 'NONE', ( #10471 ), #10572, .F. ) ;
#12635 = ORIENTED_EDGE ( 'NONE', *, *, #15342, .F. ) ;
#12636 = PRODUCT_RELATED_PRODUCT_CATEGORY ( 'part', '', ( #513 ) ) ;
#12637 = CIRCLE ( 'NONE', #4815, 60.74260934110282051 ) ;
#12638 = CARTESIAN_POINT ( 'NONE',  ( 134.3415992761220537, -66.72651222969517448, 37.22595600140377314 ) ) ;
#12639 = CARTESIAN_POINT ( 'NONE',  ( -97.49999999999997158, -190.0000000000000000, 10.00000000000000178 ) ) ;
#12640 = VERTEX_POINT ( 'NONE', #6095 ) ;
#12641 = AXIS2_PLACEMENT_3D ( 'NONE', #10128, #19248, #12987 ) ;
#12642 = ORIENTED_EDGE ( 'NONE', *, *, #3017, .F. ) ;
#12643 = ORIENTED_EDGE ( 'NONE', *, *, #6854, .T. ) ;
#12644 = FACE_OUTER_BOUND ( 'NONE', #13185, .T. ) ;
#12645 = EDGE_CURVE ( 'NONE', #648, #9091, #8439, .T. ) ;
#12646 = ORIENTED_EDGE ( 'NONE', *, *, #18038, .T. ) ;
#12647 = CARTESIAN_POINT ( 'NONE',  ( -51.77076963420845601, 31.77187437101486367, 293.5832628385307999 ) ) ;
#12648 = FACE_OUTER_BOUND ( 'NONE', #1427, .T. ) ;
#12649 = PLANE ( 'NONE',  #12022 ) ;
#12650 = PRESENTATION_STYLE_ASSIGNMENT (( #5097 ) ) ;
#12651 = DIRECTION ( 'NONE',  ( 6.982962677686266711E-15, -0.000000000000000000, 1.000000000000000000 ) ) ;
#12652 = VERTEX_POINT ( 'NONE', #13435 ) ;
#12653 = LINE ( 'NONE', #18914, #7378 ) ;
#12654 = DIRECTION ( 'NONE',  ( -0.8830229359480271656, -0.4693298356057563625, 0.000000000000000000 ) ) ;
#12655 = VECTOR ( 'NONE', #12445, 1000.000000000000000 ) ;
#12656 = ORIENTED_EDGE ( 'NONE', *, *, #4402, .F. ) ;
#12657 = CIRCLE ( 'NONE', #11674, 15.91767397667354089 ) ;
#12658 = CARTESIAN_POINT ( 'NONE',  ( -148.9554720520392834, -17.67108784863415138, 60.00000000000000000 ) ) ;
#12659 = FACE_OUTER_BOUND ( 'NONE', #13626, .T. ) ;
#12660 = EDGE_CURVE ( 'NONE', #7971, #8563, #4556, .T. ) ;
#12661 = EDGE_CURVE ( 'NONE', #3447, #6649, #1415, .T. ) ;
#12662 = CARTESIAN_POINT ( 'NONE',  ( 0.000000000000000000, 0.000000000000000000, 283.5832628385307999 ) ) ;
#12663 = CARTESIAN_POINT ( 'NONE',  ( 0.000000000000000000, 0.000000000000000000, 293.5832628385307999 ) ) ;
#12664 = DIRECTION ( 'NONE',  ( -0.000000000000000000, -0.000000000000000000, -1.000000000000000000 ) ) ;
#12665 = CARTESIAN_POINT ( 'NONE',  ( 83.45731665390675857, -124.6394201399246384, 37.68269516323560708 ) ) ;
#12666 = EDGE_CURVE ( 'NONE', #2362, #11659, #6153, .T. ) ;
#12667 = ORIENTED_EDGE ( 'NONE', *, *, #2673, .F. ) ;
#12668 = LINE ( 'NONE', #1940, #11205 ) ;
#12669 = EDGE_LOOP ( 'NONE', ( #7909, #12721, #10640, #15075 ) ) ;
#12670 = AXIS2_PLACEMENT_3D ( 'NONE', #10785, #12006, #13647 ) ;
#12671 = VERTEX_POINT ( 'NONE', #8942 ) ;
#12672 = CARTESIAN_POINT ( 'NONE',  ( -47.66508197439443961, 41.06890862491521688, 248.9926560891072143 ) ) ;
#12673 = AXIS2_PLACEMENT_3D ( 'NONE', #20004, #2730, #4156 ) ;
#12674 = ORIENTED_EDGE ( 'NONE', *, *, #3272, .T. ) ;
#12675 = CARTESIAN_POINT ( 'NONE',  ( -110.0000000000000000, 88.56916956954178488, -34.99999999999998579 ) ) ;
#12676 = CARTESIAN_POINT ( 'NONE',  ( 0.000000000000000000, 0.000000000000000000, 283.5832628385307999 ) ) ;
#12677 = VERTEX_POINT ( 'NONE', #17041 ) ;
#12678 = LINE ( 'NONE', #9204, #18838 ) ;
#12679 = CARTESIAN_POINT ( 'NONE',  ( -12.78021302872797449, 77.21438937758516374, 248.9926560891072143 ) ) ;
#12680 = VECTOR ( 'NONE', #10397, 999.9999999999998863 ) ;
#12681 = TOROIDAL_SURFACE ( 'NONE', #19549, 160.0000000000000284, 10.00000000000000000 ) ;
#12682 = DIRECTION ( 'NONE',  ( 0.7881095627315598540, 0.6155349844899715706, 0.000000000000000000 ) ) ;
#12683 = CYLINDRICAL_SURFACE ( 'NONE', #19101, 62.91752772691707207 ) ;
#12684 = AXIS2_PLACEMENT_3D ( 'NONE', #10314, #11843, #914 ) ;
#12685 = VERTEX_POINT ( 'NONE', #1282 ) ;
#12686 = CARTESIAN_POINT ( 'NONE',  ( 0.8038475772933695307, 10.39230484541327471, -5.094467845664485666E-17 ) ) ;
#12687 = FACE_OUTER_BOUND ( 'NONE', #19757, .T. ) ;
#12688 = DIRECTION ( 'NONE',  ( 1.000000000000000000, 0.000000000000000000, 0.000000000000000000 ) ) ;
#12689 = LINE ( 'NONE', #9625, #19051 ) ;
#12690 = VERTEX_POINT ( 'NONE', #15185 ) ;
#12691 = CARTESIAN_POINT ( 'NONE',  ( 42.44352287704968063, 94.20918150411493741, 14.88498244535515624 ) ) ;
#12692 = CARTESIAN_POINT ( 'NONE',  ( -74.02035518193302721, 130.4651978231461271, 22.50008790841033246 ) ) ;
#12693 = VERTEX_POINT ( 'NONE', #18162 ) ;
#12694 = ORIENTED_EDGE ( 'NONE', *, *, #4736, .F. ) ;
#12695 = ORIENTED_EDGE ( 'NONE', *, *, #15530, .T. ) ;
#12696 = VECTOR ( 'NONE', #1510, 1000.000000000000000 ) ;
#12697 = AXIS2_PLACEMENT_3D ( 'NONE', #83, #10815, #17071 ) ;
#12698 = ORIENTED_EDGE ( 'NONE', *, *, #13026, .T. ) ;
#12699 = VECTOR ( 'NONE', #12884, 1000.000000000000000 ) ;
#12700 = CARTESIAN_POINT ( 'NONE',  ( -99.31036107808984070, -131.5192173896794259, 4.249900520663169701 ) ) ;
#12701 = CARTESIAN_POINT ( 'NONE',  ( -146.8042373995521359, 31.12389395497865152, 20.84144971791933898 ) ) ;
#12702 = ORIENTED_EDGE ( 'NONE', *, *, #14786, .T. ) ;
#12703 = DIRECTION ( 'NONE',  ( -0.4338837391175643932, 0.9009688679024161484, 0.000000000000000000 ) ) ;
#12704 = CARTESIAN_POINT ( 'NONE',  ( 0.000000000000000000, 0.000000000000000000, 283.5832628385307999 ) ) ;
#12705 = CYLINDRICAL_SURFACE ( 'NONE', #10930, 7.500000000000000000 ) ;
#12706 = CARTESIAN_POINT ( 'NONE',  ( -86.69744916218965614, -122.4084679129078381, 43.21999601890001230 ) ) ;
#12707 = FACE_OUTER_BOUND ( 'NONE', #10385, .T. ) ;
#12708 = DIRECTION ( 'NONE',  ( -0.6234898018587431423, 0.7818314824680221431, 0.000000000000000000 ) ) ;
#12709 = CARTESIAN_POINT ( 'NONE',  ( -110.0000000000000142, 265.0000000000000000, 5.000000000000000888 ) ) ;
#12710 = CARTESIAN_POINT ( 'NONE',  ( 47.29944656917758294, 41.48948842197133757, 248.9926560891072143 ) ) ;
#12711 = CARTESIAN_POINT ( 'NONE',  ( -189.9999999999988916, 285.0000000000000568, 5.000000000000268230 ) ) ;
#12712 = FACE_OUTER_BOUND ( 'NONE', #7438, .T. ) ;
#12713 = DIRECTION ( 'NONE',  ( 0.5000000000000039968, 0.8660254037844362651, -3.228294802704583747E-15 ) ) ;
#12714 = AXIS2_PLACEMENT_3D ( 'NONE', #8500, #11375, #17630 ) ;
#12715 = DIRECTION ( 'NONE',  ( 0.000000000000000000, 1.000000000000000000, 3.338476886082585705E-16 ) ) ;
#12716 = VECTOR ( 'NONE', #6537, 1000.000000000000000 ) ;
#12717 = EDGE_CURVE ( 'NONE', #1375, #9156, #15279, .T. ) ;
#12718 = ORIENTED_EDGE ( 'NONE', *, *, #10361, .T. ) ;
#12719 = CARTESIAN_POINT ( 'NONE',  ( -119.5654528471588804, 59.37188176266256079, -28.72509277297836050 ) ) ;
#12720 = ORIENTED_EDGE ( 'NONE', *, *, #1271, .F. ) ;
#12721 = ORIENTED_EDGE ( 'NONE', *, *, #6045, .T. ) ;
#12722 = EDGE_CURVE ( 'NONE', #7860, #6960, #1226, .T. ) ;
#12723 = ORIENTED_EDGE ( 'NONE', *, *, #16163, .T. ) ;
#12724 = ADVANCED_FACE ( 'NONE', ( #7412 ), #18894, .T. ) ;
#12725 = AXIS2_PLACEMENT_3D ( 'NONE', #17110, #3097, #3304 ) ;
#12726 = AXIS2_PLACEMENT_3D ( 'NONE', #4047, #8653, #16539 ) ;
#12727 = EDGE_CURVE ( 'NONE', #16043, #11394, #9258, .T. ) ;
#12728 = CARTESIAN_POINT ( 'NONE',  ( 0.5584673446548692466, -5.621163452808894512, -8.263859302085696967 ) ) ;
#12729 = LINE ( 'NONE', #20198, #911 ) ;
#12730 = CARTESIAN_POINT ( 'NONE',  ( 135.7779226595531270, 102.2982297021113141, 39.99999999999999289 ) ) ;
#12731 = EDGE_LOOP ( 'NONE', ( #2261, #3319, #14213, #18596 ) ) ;
#12732 = CARTESIAN_POINT ( 'NONE',  ( 62.95000000000000284, 6.167321280506070407E-16, -5.035999999999999588 ) ) ;
#12733 = LINE ( 'NONE', #5078, #17407 ) ;
#12734 = DIRECTION ( 'NONE',  ( -0.000000000000000000, -0.000000000000000000, 1.000000000000000000 ) ) ;
#12735 = CARTESIAN_POINT ( 'NONE',  ( -7.500000000000001776, 60.00000000000000000, -105.0000000000000142 ) ) ;
#12736 = DIRECTION ( 'NONE',  ( 1.000000000000000000, 0.000000000000000000, 0.000000000000000000 ) ) ;
#12737 = EDGE_CURVE ( 'NONE', #15302, #10141, #19895, .T. ) ;
#12738 = ORIENTED_EDGE ( 'NONE', *, *, #2640, .T. ) ;
#12739 = CIRCLE ( 'NONE', #15347, 7.500000000000007105 ) ;
#12740 = CARTESIAN_POINT ( 'NONE',  ( 0.000000000000000000, 0.000000000000000000, 60.00000000000000000 ) ) ;
#12741 = AXIS2_PLACEMENT_3D ( 'NONE', #13834, #1466, #18449 ) ;
#12742 = CARTESIAN_POINT ( 'NONE',  ( 134.7088667886417284, -73.01552020433992141, 30.97729717505477609 ) ) ;
#12743 = ORIENTED_EDGE ( 'NONE', *, *, #1121, .F. ) ;
#12744 = ORIENTED_EDGE ( 'NONE', *, *, #19893, .T. ) ;
#12745 = ORIENTED_EDGE ( 'NONE', *, *, #17392, .F. ) ;
#12746 = CYLINDRICAL_SURFACE ( 'NONE', #1423, 7.500000000000001776 ) ;
#12747 = PRODUCT_DEFINITION_SHAPE ( 'NONE', 'NONE',  #20246 ) ;
#12748 = EDGE_CURVE ( 'NONE', #9808, #6926, #5890, .T. ) ;
#12749 = ORIENTED_EDGE ( 'NONE', *, *, #1979, .T. ) ;
#12750 = DIRECTION ( 'NONE',  ( -0.2080686897406943958, -0.9781142164131909622, 0.000000000000000000 ) ) ;
#12751 = ADVANCED_FACE ( 'NONE', ( #12311 ), #15627, .T. ) ;
#12752 = ADVANCED_FACE ( 'NONE', ( #19990 ), #5995, .F. ) ;
#12753 = CARTESIAN_POINT ( 'NONE',  ( -98.02376510503428619, -133.2645000753679199, 33.22592433350098418 ) ) ;
#12754 = AXIS2_PLACEMENT_3D ( 'NONE', #2164, #14728, #5428 ) ;
#12755 = CYLINDRICAL_SURFACE ( 'NONE', #10362, 10.00000000000000888 ) ;
#12756 = ORIENTED_EDGE ( 'NONE', *, *, #12964, .T. ) ;
#12757 = CIRCLE ( 'NONE', #47, 3.224098631618459443 ) ;
#12758 = CARTESIAN_POINT ( 'NONE',  ( 133.1207282269168388, -69.13111487717777948, -1.233265334176270267 ) ) ;
#12759 = CARTESIAN_POINT ( 'NONE',  ( 57.55901709132171362, 11.54977938102105028, 112.0427633081291816 ) ) ;
#12760 = ORIENTED_EDGE ( 'NONE', *, *, #19857, .T. ) ;
#12761 = CARTESIAN_POINT ( 'NONE',  ( -25.99419088092141550, 73.82206860051556419, 248.9926560891072143 ) ) ;
#12762 = CARTESIAN_POINT ( 'NONE',  ( 77.21438937758502163, 12.78021302872874010, 112.0427633081291816 ) ) ;
#12763 = PLANE ( 'NONE',  #3634 ) ;
#12764 = DIRECTION ( 'NONE',  ( -0.000000000000000000, -0.000000000000000000, 1.000000000000000000 ) ) ;
#12765 = ADVANCED_FACE ( 'NONE', ( #20095 ), #3025, .F. ) ;
#12766 = LINE ( 'NONE', #4698, #20164 ) ;
#12767 = CARTESIAN_POINT ( 'NONE',  ( 98.09575606592596841, -113.4800522715664357, 49.80233479404960661 ) ) ;
#12768 = ORIENTED_EDGE ( 'NONE', *, *, #7720, .T. ) ;
#12769 = VECTOR ( 'NONE', #2524, 1000.000000000000000 ) ;
#12770 = CYLINDRICAL_SURFACE ( 'NONE', #18416, 60.74260934110282051 ) ;
#12771 = ORIENTED_EDGE ( 'NONE', *, *, #10251, .F. ) ;
#12772 = AXIS2_PLACEMENT_3D ( 'NONE', #759, #2308, #16520 ) ;
#12773 = ORIENTED_EDGE ( 'NONE', *, *, #6486, .F. ) ;
#12774 = CARTESIAN_POINT ( 'NONE',  ( 59.30716253403183913, -13.12726406102058441, 293.5832628385307999 ) ) ;
#12775 = EDGE_CURVE ( 'NONE', #3096, #11476, #14272, .T. ) ;
#12776 = EDGE_LOOP ( 'NONE', ( #19690, #4313, #6842, #12743 ) ) ;
#12777 = EDGE_CURVE ( 'NONE', #7733, #9985, #154, .T. ) ;
#12778 = EDGE_CURVE ( 'NONE', #8041, #12677, #7434, .T. ) ;
#12779 = CARTESIAN_POINT ( 'NONE',  ( 32.61983739937762294, 51.24071425735590424, 283.5832628385307999 ) ) ;
#12780 = CARTESIAN_POINT ( 'NONE',  ( 85.53020504959901871, -140.9188050298377846, 39.99999999999999289 ) ) ;
#12781 = ORIENTED_EDGE ( 'NONE', *, *, #4048, .T. ) ;
#12782 = SURFACE_STYLE_USAGE ( .BOTH. , #6848 ) ;
#12783 = CYLINDRICAL_SURFACE ( 'NONE', #13543, 60.74260934110282051 ) ;
#12784 = DIRECTION ( 'NONE',  ( -1.000000000000000000, -0.000000000000000000, -0.000000000000000000 ) ) ;
#12785 = VECTOR ( 'NONE', #8823, 1000.000000000000000 ) ;
#12786 = FACE_BOUND ( 'NONE', #476, .T. ) ;
#12787 = LINE ( 'NONE', #805, #15365 ) ;
#12788 = CARTESIAN_POINT ( 'NONE',  ( -77.21438937758510690, -12.78021302872823384, 112.0427633081291816 ) ) ;
#12789 = VERTEX_POINT ( 'NONE', #15709 ) ;
#12790 = DIRECTION ( 'NONE',  ( 6.982962677686266711E-15, -0.000000000000000000, 1.000000000000000000 ) ) ;
#12791 = ADVANCED_FACE ( 'NONE', ( #14170 ), #11192, .T. ) ;
#12792 = CARTESIAN_POINT ( 'NONE',  ( -78.68887634719368407, -147.8252249328922687, 60.00000000000000000 ) ) ;
#12793 = CARTESIAN_POINT ( 'NONE',  ( -110.0000000000000142, 275.0000000000000000, -94.99999999999997158 ) ) ;
#12794 = CARTESIAN_POINT ( 'NONE',  ( 96.59694518724899126, -114.7646842535148153, 49.52850901074234713 ) ) ;
#12795 = ORIENTED_EDGE ( 'NONE', *, *, #17181, .T. ) ;
#12796 = LINE ( 'NONE', #14126, #8751 ) ;
#12797 = CARTESIAN_POINT ( 'NONE',  ( -69.99888493010092816, 132.6655879535290694, 4.135031488835064550 ) ) ;
#12798 = VERTEX_POINT ( 'NONE', #6404 ) ;
#12799 = EDGE_LOOP ( 'NONE', ( #17593, #2536, #5436, #7964 ) ) ;
#12800 = EDGE_LOOP ( 'NONE', ( #8043, #6480, #352, #502 ) ) ;
#12801 = APPLICATION_PROTOCOL_DEFINITION ( 'draft international standard', 'automotive_design', 1998, #14162 ) ;
#12802 = ORIENTED_EDGE ( 'NONE', *, *, #19418, .F. ) ;
#12803 = CARTESIAN_POINT ( 'NONE',  ( -97.49999999999998579, -133.9542832461881687, 40.00000000000000711 ) ) ;
#12804 = CARTESIAN_POINT ( 'NONE',  ( -135.8037181376398905, 63.74087463549686561, 35.59253210415056401 ) ) ;
#12805 = ORIENTED_EDGE ( 'NONE', *, *, #6134, .T. ) ;
#12806 = AXIS2_PLACEMENT_3D ( 'NONE', #4770, #3729, #13121 ) ;
#12807 = CYLINDRICAL_SURFACE ( 'NONE', #3776, 15.91767397667354800 ) ;
#12808 = FACE_BOUND ( 'NONE', #14165, .T. ) ;
#12809 = CARTESIAN_POINT ( 'NONE',  ( 135.1060089022256818, -65.16414933467422088, 30.00000000000000000 ) ) ;
#12810 = ADVANCED_FACE ( 'NONE', ( #12624 ), #18885, .T. ) ;
#12811 = DIRECTION ( 'NONE',  ( 0.2080686897406943681, 0.9781142164131909622, 0.000000000000000000 ) ) ;
#12812 = CARTESIAN_POINT ( 'NONE',  ( -150.0000000000000000, 0.000000000000000000, 5.000000000000011546 ) ) ;
#12813 = PLANE ( 'NONE',  #10805 ) ;
#12814 = CARTESIAN_POINT ( 'NONE',  ( 0.000000000000000000, 0.000000000000000000, 40.00000000000000000 ) ) ;
#12815 = CARTESIAN_POINT ( 'NONE',  ( 0.000000000000000000, 0.000000000000000000, 248.9926560891072143 ) ) ;
#12816 = EDGE_LOOP ( 'NONE', ( #7044, #8218, #19997, #2339 ) ) ;
#12817 = CARTESIAN_POINT ( 'NONE',  ( 7.350000000000000533, 10.39230484541327471, 0.000000000000000000 ) ) ;
#12818 = VECTOR ( 'NONE', #13946, 1000.000000000000000 ) ;
#12819 = AXIS2_PLACEMENT_3D ( 'NONE', #11961, #2574, #2778 ) ;
#12820 = ORIENTED_EDGE ( 'NONE', *, *, #8781, .T. ) ;
#12821 = VECTOR ( 'NONE', #4101, 1000.000000000000000 ) ;
#12822 = VERTEX_POINT ( 'NONE', #17456 ) ;
#12823 = ORIENTED_EDGE ( 'NONE', *, *, #12778, .T. ) ;
#12824 = CARTESIAN_POINT ( 'NONE',  ( 0.000000000000000000, 0.000000000000000000, 248.9926560891072143 ) ) ;
#12825 = EDGE_CURVE ( 'NONE', #19010, #17599, #5488, .T. ) ;
#12826 = CARTESIAN_POINT ( 'NONE',  ( 0.8038475772931082952, -5.196152422707021934, -8.999999999999998224 ) ) ;
#12827 = VECTOR ( 'NONE', #8522, 1000.000000000000000 ) ;
#12828 = DIRECTION ( 'NONE',  ( 0.000000000000000000, 0.000000000000000000, 1.000000000000000000 ) ) ;
#12829 = CIRCLE ( 'NONE', #12504, 150.0000000000000284 ) ;
#12830 = CARTESIAN_POINT ( 'NONE',  ( -11.00103590902911499, -57.65577537092155325, 112.0427633081292385 ) ) ;
#12831 = DIRECTION ( 'NONE',  ( 1.000000000000000000, 0.000000000000000000, 0.000000000000000000 ) ) ;
#12832 = CARTESIAN_POINT ( 'NONE',  ( 7.950000000000000178, 0.000000000000000000, 6.000000000000001776 ) ) ;
#12833 = LINE ( 'NONE', #8330, #2289 ) ;
#12834 = DIRECTION ( 'NONE',  ( -0.000000000000000000, -0.000000000000000000, 1.000000000000000000 ) ) ;
#12835 = FACE_OUTER_BOUND ( 'NONE', #11031, .T. ) ;
#12836 = EDGE_LOOP ( 'NONE', ( #6877, #986, #7936, #13304, #3026, #17187, #17868 ) ) ;
#12837 = EDGE_CURVE ( 'NONE', #10824, #8865, #12010, .T. ) ;
#12838 = CARTESIAN_POINT ( 'NONE',  ( 0.000000000000000000, 0.000000000000000000, 248.9926560891072143 ) ) ;
#12839 = CARTESIAN_POINT ( 'NONE',  ( 131.4992782843382031, -89.99675518205300762, 39.95150868674688382 ) ) ;
#12840 = EDGE_LOOP ( 'NONE', ( #4148, #16953 ) ) ;
#12841 = VERTEX_POINT ( 'NONE', #1893 ) ;
#12842 = AXIS2_PLACEMENT_3D ( 'NONE', #2861, #18618, #18412 ) ;
#12843 = AXIS2_PLACEMENT_3D ( 'NONE', #19356, #9943, #435 ) ;
#12844 = ORIENTED_EDGE ( 'NONE', *, *, #520, .F. ) ;
#12845 = ORIENTED_EDGE ( 'NONE', *, *, #19608, .T. ) ;
#12846 = CARTESIAN_POINT ( 'NONE',  ( -49.07263256785925876, 39.37628763770471352, 132.4711112102474146 ) ) ;
#12847 = EDGE_LOOP ( 'NONE', ( #9510, #9529, #1040, #2945, #9094 ) ) ;
#12848 = CARTESIAN_POINT ( 'NONE',  ( 60.47951622432751151, 49.67518383744852883, 132.4711112102474146 ) ) ;
#12849 = CIRCLE ( 'NONE', #4028, 15.91767397667355510 ) ;
#12850 = EDGE_CURVE ( 'NONE', #4753, #16956, #12729, .T. ) ;
#12851 = DIRECTION ( 'NONE',  ( 1.000000000000000000, 0.000000000000000000, 0.000000000000000000 ) ) ;
#12852 = EDGE_CURVE ( 'NONE', #17320, #6137, #4661, .T. ) ;
#12853 = PLANE ( 'NONE',  #15490 ) ;
#12854 = VECTOR ( 'NONE', #13700, 999.9999999999998863 ) ;
#12855 = DIRECTION ( 'NONE',  ( -0.9902903945359624593, -0.1390141521205945918, 0.000000000000000000 ) ) ;
#12856 = ORIENTED_EDGE ( 'NONE', *, *, #9093, .T. ) ;
#12857 = CARTESIAN_POINT ( 'NONE',  ( 135.1060089022257102, -65.16414933467427772, 8.535171964306037751 ) ) ;
#12858 = CARTESIAN_POINT ( 'NONE',  ( 0.000000000000000000, 0.000000000000000000, 83.57543755549745867 ) ) ;
#12859 = ORIENTED_EDGE ( 'NONE', *, *, #3500, .T. ) ;
#12860 = CARTESIAN_POINT ( 'NONE',  ( -38.35506425062487779, -44.43084819159262366, 132.4711112102474146 ) ) ;
#12861 = CARTESIAN_POINT ( 'NONE',  ( 0.000000000000000000, 0.000000000000000000, 49.99999999999999289 ) ) ;
#12862 = FACE_OUTER_BOUND ( 'NONE', #9832, .T. ) ;
#12863 = PLANE ( 'NONE',  #8322 ) ;
#12864 = EDGE_CURVE ( 'NONE', #13055, #14795, #7713, .T. ) ;
#12865 = DIRECTION ( 'NONE',  ( 1.000000000000000000, 0.000000000000000000, 0.000000000000000000 ) ) ;
#12866 = VECTOR ( 'NONE', #539, 999.9999999999998863 ) ;
#12867 = FACE_OUTER_BOUND ( 'NONE', #2194, .T. ) ;
#12868 = DIRECTION ( 'NONE',  ( 1.000000000000000000, 0.000000000000000000, -0.000000000000000000 ) ) ;
#12869 = ORIENTED_EDGE ( 'NONE', *, *, #4364, .T. ) ;
#12870 = EDGE_CURVE ( 'NONE', #14947, #3300, #350, .T. ) ;
#12871 = CARTESIAN_POINT ( 'NONE',  ( 175.7155416004667075, -197.3864744618498719, 39.99999999999998579 ) ) ;
#12872 = CIRCLE ( 'NONE', #10893, 7.500000000000020428 ) ;
#12873 = VERTEX_POINT ( 'NONE', #1690 ) ;
#12874 = VERTEX_POINT ( 'NONE', #6604 ) ;
#12875 = DIRECTION ( 'NONE',  ( -0.4338837391175651703, 0.9009688679024157043, 0.000000000000000000 ) ) ;
#12876 = ORIENTED_EDGE ( 'NONE', *, *, #5379, .F. ) ;
#12877 = DIRECTION ( 'NONE',  ( 0.000000000000000000, 1.000000000000000000, 0.000000000000000000 ) ) ;
#12878 = EDGE_CURVE ( 'NONE', #12535, #93, #14065, .T. ) ;
#12879 = ORIENTED_EDGE ( 'NONE', *, *, #10042, .T. ) ;
#12880 = VECTOR ( 'NONE', #10739, 1000.000000000000114 ) ;
#12881 = CARTESIAN_POINT ( 'NONE',  ( 138.2024300533213932, 89.85329105948596862, 49.99999999999999289 ) ) ;
#12882 = DIRECTION ( 'NONE',  ( 0.000000000000000000, 0.000000000000000000, 1.000000000000000000 ) ) ;
#12883 = CARTESIAN_POINT ( 'NONE',  ( 4.189777606611760026E-13, -60.00000000000000000, -105.0000000000000142 ) ) ;
#12884 = DIRECTION ( 'NONE',  ( -0.000000000000000000, -0.000000000000000000, -1.000000000000000000 ) ) ;
#12885 = FACE_OUTER_BOUND ( 'NONE', #305, .T. ) ;
#12886 = CARTESIAN_POINT ( 'NONE',  ( 56.12853591711344592, -23.22718332831461652, 293.5832628385307999 ) ) ;
#12887 = CARTESIAN_POINT ( 'NONE',  ( 62.95000000000000284, 0.000000000000000000, 5.035999999999999588 ) ) ;
#12888 = FACE_OUTER_BOUND ( 'NONE', #9516, .T. ) ;
#12889 = EDGE_CURVE ( 'NONE', #2638, #182, #4504, .T. ) ;
#12890 = DIRECTION ( 'NONE',  ( 0.000000000000000000, 0.000000000000000000, -1.000000000000000000 ) ) ;
#12891 = CARTESIAN_POINT ( 'NONE',  ( 95.54911406155098064, -115.6381493486011038, 49.24202537208733332 ) ) ;
#12892 = ORIENTED_EDGE ( 'NONE', *, *, #9117, .T. ) ;
#12893 = EDGE_CURVE ( 'NONE', #2439, #19124, #19861, .T. ) ;
#12894 = DIRECTION ( 'NONE',  ( -0.9396926207859068736, -0.3420201433256725987, -0.000000000000000000 ) ) ;
#12895 = CARTESIAN_POINT ( 'NONE',  ( -75.70966155199126035, 129.4926211727434691, 25.61389564976846955 ) ) ;
#12896 = ORIENTED_EDGE ( 'NONE', *, *, #8971, .T. ) ;
#12897 = AXIS2_PLACEMENT_3D ( 'NONE', #7398, #7301, #2810 ) ;
#12898 = ORIENTED_EDGE ( 'NONE', *, *, #15405, .T. ) ;
#12899 = ORIENTED_EDGE ( 'NONE', *, *, #14168, .T. ) ;
#12900 = APPLICATION_PROTOCOL_DEFINITION ( 'draft international standard', 'automotive_design', 1998, #4634 ) ;
#12901 = VERTEX_POINT ( 'NONE', #17246 ) ;
#12902 = EDGE_CURVE ( 'NONE', #13894, #15468, #1486, .T. ) ;
#12903 = CARTESIAN_POINT ( 'NONE',  ( -141.9765511393755730, 48.62330750269219237, 29.16259186082552191 ) ) ;
#12904 = ORIENTED_EDGE ( 'NONE', *, *, #16801, .T. ) ;
#12905 = VECTOR ( 'NONE', #12882, 1000.000000000000000 ) ;
#12906 = SURFACE_STYLE_FILL_AREA ( #6686 ) ;
#12907 = CARTESIAN_POINT ( 'NONE',  ( -78.85162031257831927, -85.37653928070189124, 39.88498244535600890 ) ) ;
#12908 = CARTESIAN_POINT ( 'NONE',  ( -97.78884382572438483, -133.5751867743630612, 7.606766122678530806 ) ) ;
#12909 = VECTOR ( 'NONE', #16716, 999.9999999999998863 ) ;
#12910 = CARTESIAN_POINT ( 'NONE',  ( 24.95276293194433492, -10.68636129284900704, 14.88498244535527881 ) ) ;
#12911 = DIRECTION ( 'NONE',  ( 1.000000000000000000, 0.000000000000000000, 0.000000000000000000 ) ) ;
#12912 = EDGE_CURVE ( 'NONE', #18654, #1634, #3328, .T. ) ;
#12913 = ADVANCED_FACE ( 'NONE', ( #7917 ), #9360, .F. ) ;
#12914 = DIRECTION ( 'NONE',  ( 0.6155349844899715706, -0.7881095627315598540, 0.000000000000000000 ) ) ;
#12915 = CARTESIAN_POINT ( 'NONE',  ( 0.000000000000000000, 0.000000000000000000, 49.99999999999999289 ) ) ;
#12916 = DIRECTION ( 'NONE',  ( 1.000000000000000000, 0.000000000000000000, 0.000000000000000000 ) ) ;
#12917 = EDGE_LOOP ( 'NONE', ( #1512, #2708, #2579, #19436 ) ) ;
#12918 = PRODUCT_DEFINITION_SHAPE ( 'NONE', 'NONE',  #17155 ) ;
#12919 = CARTESIAN_POINT ( 'NONE',  ( -139.8142396999972732, 3.521345544950314377, -13.33333333333314918 ) ) ;
#12920 = AXIS2_PLACEMENT_3D ( 'NONE', #3966, #11925, #5512 ) ;
#12921 = ADVANCED_FACE ( 'NONE', ( #9965 ), #14863, .F. ) ;
#12922 = EDGE_LOOP ( 'NONE', ( #19322, #14062, #12999, #6708 ) ) ;
#12923 = VERTEX_POINT ( 'NONE', #13313 ) ;
#12924 = ORIENTED_EDGE ( 'NONE', *, *, #2057, .T. ) ;
#12925 = CYLINDRICAL_SURFACE ( 'NONE', #2092, 7.500000000000020428 ) ;
#12926 = VECTOR ( 'NONE', #19501, 1000.000000000000000 ) ;
#12927 = CARTESIAN_POINT ( 'NONE',  ( -135.1060089022256818, -65.16414933467419246, 9.266975799117242119 ) ) ;
#12928 = LINE ( 'NONE', #2099, #276 ) ;
#12929 = CARTESIAN_POINT ( 'NONE',  ( -110.0000000000000000, 275.0000000000000000, 104.9999999999999858 ) ) ;
#12930 = CARTESIAN_POINT ( 'NONE',  ( -152.4599531637108498, -36.50981547337168109, 39.99999999999999289 ) ) ;
#12931 = CARTESIAN_POINT ( 'NONE',  ( 79.75827554147308263, 0.000000000000000000, 248.9926560891072143 ) ) ;
#12932 = DIRECTION ( 'NONE',  ( 6.982962677686266711E-15, -0.000000000000000000, 1.000000000000000000 ) ) ;
#12933 = LINE ( 'NONE', #17662, #12052 ) ;
#12934 = FACE_OUTER_BOUND ( 'NONE', #4793, .T. ) ;
#12935 = DIRECTION ( 'NONE',  ( 0.000000000000000000, 0.000000000000000000, 1.000000000000000000 ) ) ;
#12936 = ORIENTED_EDGE ( 'NONE', *, *, #11345, .T. ) ;
#12937 = DIRECTION ( 'NONE',  ( 1.000000000000000000, 0.000000000000000000, 0.000000000000000000 ) ) ;
#12938 = AXIS2_PLACEMENT_3D ( 'NONE', #18865, #6386, #15788 ) ;
#12939 = ORIENTED_EDGE ( 'NONE', *, *, #14655, .F. ) ;
#12940 = ORIENTED_EDGE ( 'NONE', *, *, #1111, .T. ) ;
#12941 = VECTOR ( 'NONE', #15419, 1000.000000000000000 ) ;
#12942 = ORIENTED_EDGE ( 'NONE', *, *, #6366, .T. ) ;
#12943 = ORIENTED_EDGE ( 'NONE', *, *, #8748, .T. ) ;
#12944 = CARTESIAN_POINT ( 'NONE',  ( 12.14914984460761360, 59.51523122377248853, 283.5832628385307999 ) ) ;
#12945 = AXIS2_PLACEMENT_3D ( 'NONE', #19123, #8662, #18174 ) ;
#12946 = ORIENTED_EDGE ( 'NONE', *, *, #4018, .F. ) ;
#12947 = CARTESIAN_POINT ( 'NONE',  ( 175.8776271403848739, -36.50981547336952104, 39.99999999999999289 ) ) ;
#12948 = CARTESIAN_POINT ( 'NONE',  ( 71.18887634719571622, -147.8252249328912740, 39.99999999999999289 ) ) ;
#12949 = LINE ( 'NONE', #13339, #6356 ) ;
#12950 = DIRECTION ( 'NONE',  ( -1.000000000000000000, 0.000000000000000000, 0.000000000000000000 ) ) ;
#12951 = EDGE_LOOP ( 'NONE', ( #1781, #721, #18196, #2048 ) ) ;
#12952 = CARTESIAN_POINT ( 'NONE',  ( 124.4476442249721941, -83.75451619235310829, -9.879193670931774918 ) ) ;
#12953 = DIRECTION ( 'NONE',  ( 0.000000000000000000, 1.000000000000000000, 0.000000000000000000 ) ) ;
#12954 = ORIENTED_EDGE ( 'NONE', *, *, #1677, .T. ) ;
#12955 = AXIS2_PLACEMENT_3D ( 'NONE', #5245, #11471, #3501 ) ;
#12956 = PLANE ( 'NONE',  #6767 ) ;
#12957 = CARTESIAN_POINT ( 'NONE',  ( -109.5721339228237667, 31.03941509555038181, 14.88498244535621851 ) ) ;
#12958 = LINE ( 'NONE', #5106, #19451 ) ;
#12959 = AXIS2_PLACEMENT_3D ( 'NONE', #14020, #5746, #11962 ) ;
#12960 = DIRECTION ( 'NONE',  ( -6.982962677686266711E-15, 0.000000000000000000, -1.000000000000000000 ) ) ;
#12961 = LINE ( 'NONE', #10102, #13787 ) ;
#12962 = CARTESIAN_POINT ( 'NONE',  ( 100.7812500000000000, -111.0996833858562525, 49.99999999999999289 ) ) ;
#12963 = ORIENTED_EDGE ( 'NONE', *, *, #896, .F. ) ;
#12964 = EDGE_CURVE ( 'NONE', #12901, #2793, #12024, .T. ) ;
#12965 = CARTESIAN_POINT ( 'NONE',  ( 56.50138340076689047, -22.29928840491054132, 283.5832628385307999 ) ) ;
#12966 = ORIENTED_EDGE ( 'NONE', *, *, #5903, .T. ) ;
#12967 = ORIENTED_EDGE ( 'NONE', *, *, #7118, .F. ) ;
#12968 = EDGE_CURVE ( 'NONE', #9508, #19079, #459, .T. ) ;
#12969 = CARTESIAN_POINT ( 'NONE',  ( 107.5000000000000142, -118.5063289449133492, 40.00000000000000000 ) ) ;
#12970 = VERTEX_POINT ( 'NONE', #8224 ) ;
#12971 = DIRECTION ( 'NONE',  ( -0.1736481776669404897, -0.9848077530122062440, 1.206153050004590509E-15 ) ) ;
#12972 = VECTOR ( 'NONE', #9297, 1000.000000000000000 ) ;
#12973 = EDGE_CURVE ( 'NONE', #17837, #13913, #11595, .T. ) ;
#12974 = CARTESIAN_POINT ( 'NONE',  ( -0.7000608949449729224, -5.693982670708925831, 293.5832628385307999 ) ) ;
#12975 = VECTOR ( 'NONE', #13840, 1000.000000000000227 ) ;
#12976 = EDGE_CURVE ( 'NONE', #18905, #18064, #12928, .T. ) ;
#12977 = CARTESIAN_POINT ( 'NONE',  ( -3.931715182917647021E-15, -8.014718854569428785, -4.118099735505511561 ) ) ;
#12978 = DIRECTION ( 'NONE',  ( 0.000000000000000000, 0.000000000000000000, -1.000000000000000000 ) ) ;
#12979 = EDGE_CURVE ( 'NONE', #17599, #5045, #10067, .T. ) ;
#12980 = DIRECTION ( 'NONE',  ( -1.000000000000000000, 0.000000000000000000, 0.000000000000000000 ) ) ;
#12981 = CARTESIAN_POINT ( 'NONE',  ( 101.1837452960046875, -128.8430157189652618, 2.240558877795664205 ) ) ;
#12982 = CARTESIAN_POINT ( 'NONE',  ( 56.84754764479241373, -154.7316448359447634, 60.00000000000000000 ) ) ;
#12983 = DIRECTION ( 'NONE',  ( -2.775557561562892929E-15, -1.000000000000000000, -1.734723475976808080E-16 ) ) ;
#12984 = ORIENTED_EDGE ( 'NONE', *, *, #10737, .F. ) ;
#12985 = CARTESIAN_POINT ( 'NONE',  ( 0.000000000000000000, 0.000000000000000000, 283.5832628385307999 ) ) ;
#12986 = APPLICATION_CONTEXT ( 'automotive_design' ) ;
#12987 = DIRECTION ( 'NONE',  ( -1.000000000000000000, 0.000000000000000000, 0.000000000000000000 ) ) ;
#12988 = CARTESIAN_POINT ( 'NONE',  ( 82.76227416097492551, -125.1020663115147755, 4.285849343614037465 ) ) ;
#12989 = CARTESIAN_POINT ( 'NONE',  ( 93.97987429418127192, -116.9112352313885026, 48.64721126355986058 ) ) ;
#12990 = CIRCLE ( 'NONE', #14936, 112.8770930172170068 ) ;
#12991 = EDGE_LOOP ( 'NONE', ( #1712, #13815, #12845, #16811 ) ) ;
#12992 = EDGE_CURVE ( 'NONE', #3335, #19683, #13215, .T. ) ;
#12993 = VECTOR ( 'NONE', #2884, 1000.000000000000000 ) ;
#12994 = CARTESIAN_POINT ( 'NONE',  ( -1.379293853801755176, 58.69016442926522359, 132.4711112102474146 ) ) ;
#12995 = CARTESIAN_POINT ( 'NONE',  ( -75.26293162660911662, 129.7525693666177915, 24.85252474122213684 ) ) ;
#12996 = ORIENTED_EDGE ( 'NONE', *, *, #3283, .T. ) ;
#12997 = ORIENTED_EDGE ( 'NONE', *, *, #6252, .F. ) ;
#12998 = EDGE_LOOP ( 'NONE', ( #17824, #7673, #16007, #20214 ) ) ;
#12999 = ORIENTED_EDGE ( 'NONE', *, *, #11146, .T. ) ;
#13000 = LINE ( 'NONE', #8403, #15322 ) ;
#13001 = CARTESIAN_POINT ( 'NONE',  ( -138.1756879020936424, 58.38534797887673733, 33.39972604561270941 ) ) ;
#13002 = VERTEX_POINT ( 'NONE', #16415 ) ;
#13003 = EDGE_CURVE ( 'NONE', #18698, #7038, #8115, .T. ) ;
#13004 = DIRECTION ( 'NONE',  ( -0.000000000000000000, -1.000000000000000000, -0.000000000000000000 ) ) ;
#13005 = DIRECTION ( 'NONE',  ( -0.000000000000000000, -0.000000000000000000, 1.000000000000000000 ) ) ;
#13006 = CARTESIAN_POINT ( 'NONE',  ( -82.95463716431548562, -124.9741831325247148, 3.790176040462246654 ) ) ;
#13007 = ORIENTED_EDGE ( 'NONE', *, *, #13616, .T. ) ;
#13008 = VECTOR ( 'NONE', #8124, 1000.000000000000000 ) ;
#13009 = ADVANCED_FACE ( 'NONE', ( #14671 ), #12681, .F. ) ;
#13010 = VECTOR ( 'NONE', #13479, 1000.000000000000000 ) ;
#13011 = CARTESIAN_POINT ( 'NONE',  ( 48.17959877923549072, 36.99514631729036296, 283.5832628385307999 ) ) ;
#13012 = DIRECTION ( 'NONE',  ( -0.000000000000000000, -1.000000000000000000, -0.000000000000000000 ) ) ;
#13013 = CARTESIAN_POINT ( 'NONE',  ( 56.84754764479240663, -154.7316448359447634, 39.99999999999999289 ) ) ;
#13014 = DIRECTION ( 'NONE',  ( -0.000000000000000000, -0.000000000000000000, 1.000000000000000000 ) ) ;
#13015 = DIRECTION ( 'NONE',  ( 0.000000000000000000, 0.000000000000000000, 1.000000000000000000 ) ) ;
#13016 = ORIENTED_EDGE ( 'NONE', *, *, #3274, .T. ) ;
#13017 = ADVANCED_FACE ( 'NONE', ( #19479 ), #16318, .F. ) ;
#13018 = CARTESIAN_POINT ( 'NONE',  ( 0.8038475772931082952, -5.196152422707021934, -8.999999999999998224 ) ) ;
#13019 = AXIS2_PLACEMENT_3D ( 'NONE', #3768, #16064, #2046 ) ;
#13020 = VECTOR ( 'NONE', #9860, 1000.000000000000000 ) ;
#13021 = ORIENTED_EDGE ( 'NONE', *, *, #14979, .T. ) ;
#13022 = ORIENTED_EDGE ( 'NONE', *, *, #8774, .T. ) ;
#13023 = VERTEX_POINT ( 'NONE', #5177 ) ;
#13024 = EDGE_CURVE ( 'NONE', #11048, #18614, #8532, .T. ) ;
#13025 = CARTESIAN_POINT ( 'NONE',  ( 12.78021302872850562, -77.21438937758507848, 112.0427633081291816 ) ) ;
#13026 = EDGE_CURVE ( 'NONE', #11442, #7743, #17953, .T. ) ;
#13027 = CARTESIAN_POINT ( 'NONE',  ( -134.6604885881914413, -66.08112487034745186, 4.281233480891749821 ) ) ;
#13028 = CARTESIAN_POINT ( 'NONE',  ( 47.56406379474552182, 37.78325588002191893, 293.5832628385307999 ) ) ;
#13029 = DIRECTION ( 'NONE',  ( -0.000000000000000000, -0.000000000000000000, 1.000000000000000000 ) ) ;
#13030 = VECTOR ( 'NONE', #5000, 1000.000000000000000 ) ;
#13031 = EDGE_CURVE ( 'NONE', #7290, #10780, #1918, .T. ) ;
#13032 = EDGE_LOOP ( 'NONE', ( #18941, #19296, #11821, #13947 ) ) ;
#13033 = LINE ( 'NONE', #17561, #13338 ) ;
#13034 = VECTOR ( 'NONE', #4123, 1000.000000000000114 ) ;
#13035 = CARTESIAN_POINT ( 'NONE',  ( 132.9399949862693404, -69.60197982539588679, 6.632446261229627993 ) ) ;
#13036 = CARTESIAN_POINT ( 'NONE',  ( 19.74955734592081669, 8.656064874777317897, 248.9926560891072143 ) ) ;
#13037 = EDGE_CURVE ( 'NONE', #2316, #18758, #848, .T. ) ;
#13038 = CARTESIAN_POINT ( 'NONE',  ( 99.31036107808986912, -131.5192173896793690, 35.75009947933683208 ) ) ;
#13039 = DIRECTION ( 'NONE',  ( -1.000000000000000000, 0.000000000000000000, 0.000000000000000000 ) ) ;
#13040 = ORIENTED_EDGE ( 'NONE', *, *, #11997, .T. ) ;
#13041 = ORIENTED_EDGE ( 'NONE', *, *, #6092, .F. ) ;
#13042 = ORIENTED_EDGE ( 'NONE', *, *, #5, .T. ) ;
#13043 = EDGE_LOOP ( 'NONE', ( #11465, #15769 ) ) ;
#13044 = CIRCLE ( 'NONE', #4224, 32.50000000000000000 ) ;
#13045 = VECTOR ( 'NONE', #16936, 1000.000000000000114 ) ;
#13046 = ORIENTED_EDGE ( 'NONE', *, *, #5021, .F. ) ;
#13047 = ORIENTED_EDGE ( 'NONE', *, *, #4532, .F. ) ;
#13048 = DIRECTION ( 'NONE',  ( 1.000000000000000000, 0.000000000000000000, 0.000000000000000000 ) ) ;
#13049 = DIRECTION ( 'NONE',  ( -0.4999999999999919509, -0.8660254037844432595, 0.000000000000000000 ) ) ;
#13050 = DIRECTION ( 'NONE',  ( 0.000000000000000000, 0.000000000000000000, 1.000000000000000000 ) ) ;
#13051 = VERTEX_POINT ( 'NONE', #3724 ) ;
#13052 = LINE ( 'NONE', #13239, #1500 ) ;
#13053 = CARTESIAN_POINT ( 'NONE',  ( 21.51662357877997422, -16.14275151819498078, 14.88498244535530191 ) ) ;
#13054 = EDGE_CURVE ( 'NONE', #7743, #10155, #3922, .T. ) ;
#13055 = VERTEX_POINT ( 'NONE', #5366 ) ;
#13056 = CARTESIAN_POINT ( 'NONE',  ( -106.6474863415760979, 92.74702262351860327, -34.89460852530158519 ) ) ;
#13057 = DIRECTION ( 'NONE',  ( 0.7660444431189835646, -0.6427876096865328126, 0.000000000000000000 ) ) ;
#13058 = CYLINDRICAL_SURFACE ( 'NONE', #8199, 7.500000000000020428 ) ;
#13059 = CARTESIAN_POINT ( 'NONE',  ( 92.34802049131702972, -66.64338626758360817, 39.88498244535480808 ) ) ;
#13060 = DIRECTION ( 'NONE',  ( -0.000000000000000000, 0.000000000000000000, -1.000000000000000000 ) ) ;
#13061 = CARTESIAN_POINT ( 'NONE',  ( -54.86954475316242252, 20.84572577951219330, 111.4180192758973931 ) ) ;
#13062 = ORIENTED_EDGE ( 'NONE', *, *, #15819, .F. ) ;
#13063 = DIRECTION ( 'NONE',  ( 0.000000000000000000, -0.5000000000000018874, -0.8660254037844374864 ) ) ;
#13064 = EDGE_LOOP ( 'NONE', ( #3195, #941 ) ) ;
#13065 = VERTEX_POINT ( 'NONE', #3823 ) ;
#13066 = VECTOR ( 'NONE', #14311, 1000.000000000000000 ) ;
#13067 = DIRECTION ( 'NONE',  ( 0.5000000000000039968, -0.8660254037844363761, 0.000000000000000000 ) ) ;
#13068 = EDGE_LOOP ( 'NONE', ( #5038, #11188, #7070 ) ) ;
#13069 = AXIS2_PLACEMENT_3D ( 'NONE', #17511, #5030, #8076 ) ;
#13070 = CARTESIAN_POINT ( 'NONE',  ( 0.000000000000000000, 0.000000000000000000, 283.5832628385307999 ) ) ;
#13071 = CARTESIAN_POINT ( 'NONE',  ( -85.34080972464063564, -123.3578596465555819, 41.36707920009423844 ) ) ;
#13072 = CARTESIAN_POINT ( 'NONE',  ( 48.89172014028660129, 94.20918150411493741, 14.88498244535511184 ) ) ;
#13073 = DIRECTION ( 'NONE',  ( 0.000000000000000000, 0.000000000000000000, -1.000000000000000000 ) ) ;
#13074 = EDGE_CURVE ( 'NONE', #6267, #11201, #7099, .T. ) ;
#13075 = EDGE_LOOP ( 'NONE', ( #3218, #6298, #7382, #5806 ) ) ;
#13076 = DIRECTION ( 'NONE',  ( 6.982962677686266711E-15, -0.000000000000000000, 1.000000000000000000 ) ) ;
#13077 = DIRECTION ( 'NONE',  ( 0.000000000000000000, 0.000000000000000000, 1.000000000000000000 ) ) ;
#13078 = LINE ( 'NONE', #17905, #19947 ) ;
#13079 = CARTESIAN_POINT ( 'NONE',  ( 41.06890862491472660, 47.66508197439486594, 248.9926560891072143 ) ) ;
#13080 = ORIENTED_EDGE ( 'NONE', *, *, #20235, .F. ) ;
#13081 = DIRECTION ( 'NONE',  ( 0.9271237148521548344, -0.3747554100459928317, 0.000000000000000000 ) ) ;
#13082 = CARTESIAN_POINT ( 'NONE',  ( 73.82206860051529418, 25.99419088092216867, 111.4180192758973362 ) ) ;
#13083 = CARTESIAN_POINT ( 'NONE',  ( 92.20932192393671301, -118.3126747524535602, -7.798439241158999558 ) ) ;
#13084 = VECTOR ( 'NONE', #18691, 1000.000000000000000 ) ;
#13085 = CARTESIAN_POINT ( 'NONE',  ( -4.581103194068993467, 3.453261854572370559, 293.5832628385307999 ) ) ;
#13086 = ORIENTED_EDGE ( 'NONE', *, *, #7162, .F. ) ;
#13087 = ADVANCED_FACE ( 'NONE', ( #16014 ), #1998, .F. ) ;
#13088 = CARTESIAN_POINT ( 'NONE',  ( 63.68887634719570912, -147.8252249328912740, 49.99999999999999289 ) ) ;
#13089 = DIRECTION ( 'NONE',  ( 1.000000000000000000, 0.000000000000000000, -6.994638739193269649E-15 ) ) ;
#13090 = ORIENTED_EDGE ( 'NONE', *, *, #9852, .F. ) ;
#13091 = ORIENTED_EDGE ( 'NONE', *, *, #10481, .F. ) ;
#13092 = ORIENTED_EDGE ( 'NONE', *, *, #8660, .T. ) ;
#13093 = APPLICATION_PROTOCOL_DEFINITION ( 'draft international standard', 'automotive_design', 1998, #16261 ) ;
#13094 = CARTESIAN_POINT ( 'NONE',  ( 61.81362617575102547, -11.73417718768070372, 293.5832628385307999 ) ) ;
#13095 = VECTOR ( 'NONE', #4152, 1000.000000000000000 ) ;
#13096 = CARTESIAN_POINT ( 'NONE',  ( 0.000000000000000000, 0.000000000000000000, 49.99999999999999289 ) ) ;
#13097 = VERTEX_POINT ( 'NONE', #7588 ) ;
#13098 = PLANE ( 'NONE',  #5095 ) ;
#13099 = CARTESIAN_POINT ( 'NONE',  ( -37.78198917157317993, 47.56244194535177883, 283.5832628385307999 ) ) ;
#13100 = CARTESIAN_POINT ( 'NONE',  ( -97.37676942331958685, -115.5300780475897398, 10.30568642992988515 ) ) ;
#13101 = EDGE_CURVE ( 'NONE', #7659, #12671, #15371, .T. ) ;
#13102 = CARTESIAN_POINT ( 'NONE',  ( -24.73834469112697576, -10.56256686379325593, 14.88498244535562520 ) ) ;
#13103 = FACE_OUTER_BOUND ( 'NONE', #10854, .T. ) ;
#13104 = LINE ( 'NONE', #9950, #1382 ) ;
#13105 = LINE ( 'NONE', #932, #10100 ) ;
#13106 = DIRECTION ( 'NONE',  ( 6.982962677686266711E-15, 0.000000000000000000, 1.000000000000000000 ) ) ;
#13107 = ORIENTED_EDGE ( 'NONE', *, *, #19754, .T. ) ;
#13108 = EDGE_CURVE ( 'NONE', #16722, #18380, #20074, .T. ) ;
#13109 = DIRECTION ( 'NONE',  ( -0.000000000000000000, -0.000000000000000000, 1.000000000000000000 ) ) ;
#13110 = ADVANCED_FACE ( 'NONE', ( #13831 ), #4221, .F. ) ;
#13111 = ORIENTED_EDGE ( 'NONE', *, *, #13114, .F. ) ;
#13112 = EDGE_LOOP ( 'NONE', ( #16516, #9347 ) ) ;
#13113 = LINE ( 'NONE', #9759, #8928 ) ;
#13114 = EDGE_CURVE ( 'NONE', #2315, #17279, #7292, .T. ) ;
#13115 = CARTESIAN_POINT ( 'NONE',  ( -123.6381990918736449, -84.94542618836281633, -9.999999999999998224 ) ) ;
#13116 = CARTESIAN_POINT ( 'NONE',  ( -97.77191798235034526, 62.82820655979934088, 39.88498244535613679 ) ) ;
#13117 = DIRECTION ( 'NONE',  ( -0.9396926207859104263, 0.3420201433256630508, 0.000000000000000000 ) ) ;
#13118 = CARTESIAN_POINT ( 'NONE',  ( -135.3391293778863087, -31.30995385105789808, -18.16960702786510140 ) ) ;
#13119 = DIRECTION ( 'NONE',  ( 1.000000000000000000, 0.000000000000000000, 0.000000000000000000 ) ) ;
#13120 = CARTESIAN_POINT ( 'NONE',  ( -133.5342034995409790, -80.71481093437574827, 2.145336860065035989 ) ) ;
#13121 = DIRECTION ( 'NONE',  ( 1.000000000000000000, 0.000000000000000000, -6.977185866873308817E-15 ) ) ;
#13122 = CYLINDRICAL_SURFACE ( 'NONE', #6585, 7.500000000000001776 ) ;
#13123 = PLANE ( 'NONE',  #572 ) ;
#13124 = PRODUCT_DEFINITION_CONTEXT ( 'detailed design', #17313, 'design' ) ;
#13125 = VERTEX_POINT ( 'NONE', #16808 ) ;
#13126 = EDGE_CURVE ( 'NONE', #2863, #3875, #16911, .T. ) ;
#13127 = EDGE_CURVE ( 'NONE', #4551, #7267, #15292, .T. ) ;
#13128 = EDGE_CURVE ( 'NONE', #347, #18954, #9022, .T. ) ;
#13129 = EDGE_CURVE ( 'NONE', #2720, #6700, #16707, .T. ) ;
#13130 = VERTEX_POINT ( 'NONE', #12191 ) ;
#13131 = ORIENTED_EDGE ( 'NONE', *, *, #478, .T. ) ;
#13132 = ORIENTED_EDGE ( 'NONE', *, *, #15155, .T. ) ;
#13133 = CARTESIAN_POINT ( 'NONE',  ( 18.28503710798548454, -57.92514141135459482, 283.5832628385307999 ) ) ;
#13134 = AXIS2_PLACEMENT_3D ( 'NONE', #15801, #14366, #3716 ) ;
#13135 = AXIS2_PLACEMENT_3D ( 'NONE', #9820, #5325, #6859 ) ;
#13136 = EDGE_LOOP ( 'NONE', ( #7192, #13163 ) ) ;
#13137 = EDGE_CURVE ( 'NONE', #18566, #17239, #18247, .T. ) ;
#13138 = DIRECTION ( 'NONE',  ( 0.000000000000000000, 0.000000000000000000, 1.000000000000000000 ) ) ;
#13139 = CARTESIAN_POINT ( 'NONE',  ( 122.8001410695374744, -86.14014948502065749, 49.99999999999999289 ) ) ;
#13140 = EDGE_CURVE ( 'NONE', #13775, #3366, #12296, .T. ) ;
#13141 = DIRECTION ( 'NONE',  ( -6.982962677686266711E-15, 0.000000000000000000, -1.000000000000000000 ) ) ;
#13142 = ORIENTED_EDGE ( 'NONE', *, *, #19604, .F. ) ;
#13143 = AXIS2_PLACEMENT_3D ( 'NONE', #7755, #7859, #13687 ) ;
#13144 = DIRECTION ( 'NONE',  ( -0.8479630283625716469, 0.5300553768524345344, 0.000000000000000000 ) ) ;
#13145 = LINE ( 'NONE', #17685, #12716 ) ;
#13146 = VERTEX_POINT ( 'NONE', #8921 ) ;
#13147 = CARTESIAN_POINT ( 'NONE',  ( 0.000000000000000000, 0.000000000000000000, 283.5832628385307999 ) ) ;
#13148 = LINE ( 'NONE', #5397, #7725 ) ;
#13149 = DIRECTION ( 'NONE',  ( 0.000000000000000000, 0.000000000000000000, 1.000000000000000000 ) ) ;
#13150 = DIRECTION ( 'NONE',  ( 1.000000000000000000, 0.000000000000000000, 0.000000000000000000 ) ) ;
#13151 = AXIS2_PLACEMENT_3D ( 'NONE', #16595, #2482, #936 ) ;
#13152 = EDGE_CURVE ( 'NONE', #13130, #11373, #9435, .T. ) ;
#13153 = DIRECTION ( 'NONE',  ( -1.000000000000000000, 0.000000000000000000, 6.994638739193269649E-15 ) ) ;
#13154 = CARTESIAN_POINT ( 'NONE',  ( -85.53020504959707182, -140.9188050298390067, 39.99999999999999289 ) ) ;
#13155 = DIRECTION ( 'NONE',  ( 1.000000000000000000, 0.000000000000000000, 0.000000000000000000 ) ) ;
#13156 = ORIENTED_EDGE ( 'NONE', *, *, #18508, .T. ) ;
#13157 = DIRECTION ( 'NONE',  ( 0.000000000000000000, 0.000000000000000000, -1.000000000000000000 ) ) ;
#13158 = VERTEX_POINT ( 'NONE', #2901 ) ;
#13159 = CIRCLE ( 'NONE', #8912, 7.500000000000007105 ) ;
#13160 = EDGE_CURVE ( 'NONE', #14365, #1787, #4197, .T. ) ;
#13161 = ORIENTED_EDGE ( 'NONE', *, *, #3259, .T. ) ;
#13162 = DIRECTION ( 'NONE',  ( 0.000000000000000000, 0.000000000000000000, 1.000000000000000000 ) ) ;
#13163 = ORIENTED_EDGE ( 'NONE', *, *, #5936, .F. ) ;
#13164 = DIRECTION ( 'NONE',  ( -0.6234898018587424762, 0.7818314824680228092, 0.000000000000000000 ) ) ;
#13165 = CARTESIAN_POINT ( 'NONE',  ( 15.91767397667354089, 149.1530343478547422, 49.99999999999999289 ) ) ;
#13166 = VECTOR ( 'NONE', #19225, 1000.000000000000227 ) ;
#13167 = FACE_BOUND ( 'NONE', #1012, .T. ) ;
#13168 = DIRECTION ( 'NONE',  ( -0.000000000000000000, -0.000000000000000000, 1.000000000000000000 ) ) ;
#13169 = ORIENTED_EDGE ( 'NONE', *, *, #15761, .F. ) ;
#13170 = CARTESIAN_POINT ( 'NONE',  ( 15.91767397667354089, 149.1530343478547422, 49.99999999999999289 ) ) ;
#13171 = CARTESIAN_POINT ( 'NONE',  ( 98.51475352695847221, -132.6070668284232568, 5.590591466758980665 ) ) ;
#13172 = AXIS2_PLACEMENT_3D ( 'NONE', #1041, #18444, #7384 ) ;
#13173 = LINE ( 'NONE', #16568, #16359 ) ;
#13174 = PLANE ( 'NONE',  #8658 ) ;
#13175 = VERTEX_POINT ( 'NONE', #9127 ) ;
#13176 = VECTOR ( 'NONE', #14088, 1000.000000000000000 ) ;
#13177 = LINE ( 'NONE', #809, #14288 ) ;
#13178 = DIRECTION ( 'NONE',  ( 1.000000000000000000, 0.000000000000000000, 0.000000000000000000 ) ) ;
#13179 = CARTESIAN_POINT ( 'NONE',  ( 11.73417718768048701, 61.81362617575105389, 293.5832628385307999 ) ) ;
#13180 = ORIENTED_EDGE ( 'NONE', *, *, #9252, .T. ) ;
#13181 = DIRECTION ( 'NONE',  ( 0.5000000000000039968, 0.8660254037844363761, -3.491481338843161754E-15 ) ) ;
#13182 = FACE_OUTER_BOUND ( 'NONE', #4226, .T. ) ;
#13183 = AXIS2_PLACEMENT_3D ( 'NONE', #17415, #15670, #17315 ) ;
#13184 = VERTEX_POINT ( 'NONE', #5664 ) ;
#13185 = EDGE_LOOP ( 'NONE', ( #18311, #13156, #8202, #6013 ) ) ;
#13186 = AXIS2_PLACEMENT_3D ( 'NONE', #2573, #10148, #14843 ) ;
#13187 = CARTESIAN_POINT ( 'NONE',  ( -136.4994460260996902, -31.11111111111111782, -9.999999999999987566 ) ) ;
#13188 = DIRECTION ( 'NONE',  ( 0.000000000000000000, 0.000000000000000000, -1.000000000000000000 ) ) ;
#13189 = VECTOR ( 'NONE', #5685, 1000.000000000000000 ) ;
#13190 = EDGE_LOOP ( 'NONE', ( #5916, #6436, #11903, #15617 ) ) ;
#13191 = FACE_OUTER_BOUND ( 'NONE', #5753, .T. ) ;
#13192 = CARTESIAN_POINT ( 'NONE',  ( 0.01899995639453659624, 8.236198097127171991, 3.734486434573634828 ) ) ;
#13193 = CARTESIAN_POINT ( 'NONE',  ( -99.06221739375143898, -131.8607669219689171, 4.630169983262292455 ) ) ;
#13194 = ORIENTED_EDGE ( 'NONE', *, *, #5302, .F. ) ;
#13195 = CARTESIAN_POINT ( 'NONE',  ( -137.0737990618249853, -28.59114739397107741, 27.19870260277823348 ) ) ;
#13196 = DIRECTION ( 'NONE',  ( -1.000000000000000000, 0.000000000000000000, 0.000000000000000000 ) ) ;
#13197 = CARTESIAN_POINT ( 'NONE',  ( 1.379293853801755176, -78.26059000578310076, 248.9926560891072143 ) ) ;
#13198 = CARTESIAN_POINT ( 'NONE',  ( -159.9599531637108782, -36.50981547337168109, 39.99999999999999289 ) ) ;
#13199 = VECTOR ( 'NONE', #5231, 1000.000000000000000 ) ;
#13200 = CARTESIAN_POINT ( 'NONE',  ( 28.15057869795588985, 51.51682027493075111, 132.4711112102474146 ) ) ;
#13201 = CARTESIAN_POINT ( 'NONE',  ( -78.26059000578311498, 0.8220851292432594937, 248.9926560891072143 ) ) ;
#13202 = DIRECTION ( 'NONE',  ( 1.000000000000000000, 0.000000000000000000, -6.994638739193269649E-15 ) ) ;
#13203 = ORIENTED_EDGE ( 'NONE', *, *, #9894, .T. ) ;
#13204 = CARTESIAN_POINT ( 'NONE',  ( -109.9999999999983515, 285.0000000000000568, 77.50000000000000000 ) ) ;
#13205 = CARTESIAN_POINT ( 'NONE',  ( 17.50000000000001066, 0.000000000000000000, 293.5832628385307999 ) ) ;
#13206 = ADVANCED_FACE ( 'NONE', ( #10553 ), #6388, .F. ) ;
#13207 = VECTOR ( 'NONE', #9615, 1000.000000000000000 ) ;
#13208 = ORIENTED_EDGE ( 'NONE', *, *, #3109, .F. ) ;
#13209 = ORIENTED_EDGE ( 'NONE', *, *, #16283, .T. ) ;
#13210 = AXIS2_PLACEMENT_3D ( 'NONE', #7856, #14407, #9395 ) ;
#13211 = EDGE_CURVE ( 'NONE', #7403, #1374, #8794, .T. ) ;
#13212 = CARTESIAN_POINT ( 'NONE',  ( 159.9599531637113330, -36.50981547336952104, 49.99999999999999289 ) ) ;
#13213 = CARTESIAN_POINT ( 'NONE',  ( -132.6585078626522147, -70.01400725886476550, -2.312657259978039725 ) ) ;
#13214 = EDGE_CURVE ( 'NONE', #11944, #321, #15131, .T. ) ;
#13215 = LINE ( 'NONE', #563, #16937 ) ;
#13216 = EDGE_CURVE ( 'NONE', #4335, #2635, #16620, .T. ) ;
#13217 = CARTESIAN_POINT ( 'NONE',  ( 47.66508197439472383, -41.06890862491489003, 132.4711112102474146 ) ) ;
#13218 = DIRECTION ( 'NONE',  ( -6.982962677686266711E-15, 0.000000000000000000, -1.000000000000000000 ) ) ;
#13219 = ORIENTED_EDGE ( 'NONE', *, *, #15285, .F. ) ;
#13220 = ADVANCED_FACE ( 'NONE', ( #1018 ), #5731, .T. ) ;
#13221 = CARTESIAN_POINT ( 'NONE',  ( 0.000000000000000000, 0.000000000000000000, -115.0000000000000000 ) ) ;
#13222 = CARTESIAN_POINT ( 'NONE',  ( -131.2732777714346923, -90.85536658133409560, 4.758170025484766625E-15 ) ) ;
#13223 = DIRECTION ( 'NONE',  ( 0.000000000000000000, 0.000000000000000000, 1.000000000000000000 ) ) ;
#13224 = CARTESIAN_POINT ( 'NONE',  ( -4.811834253408968642, -3.123743752084041425, 283.5832628385307999 ) ) ;
#13225 = AXIS2_PLACEMENT_3D ( 'NONE', #604, #13168, #6849 ) ;
#13226 = CARTESIAN_POINT ( 'NONE',  ( -29.99999999999887379, 275.0000000000000000, 4.999999999999158007 ) ) ;
#13227 = EDGE_LOOP ( 'NONE', ( #6068, #17350, #12563, #900 ) ) ;
#13228 = EDGE_CURVE ( 'NONE', #8156, #11394, #6143, .T. ) ;
#13229 = ORIENTED_EDGE ( 'NONE', *, *, #13140, .T. ) ;
#13230 = ORIENTED_EDGE ( 'NONE', *, *, #3668, .F. ) ;
#13231 = CIRCLE ( 'NONE', #1824, 127.4413876050234649 ) ;
#13232 = VERTEX_POINT ( 'NONE', #11945 ) ;
#13233 = EDGE_LOOP ( 'NONE', ( #3420, #14491, #7145, #4968 ) ) ;
#13234 = CARTESIAN_POINT ( 'NONE',  ( -79.75827554147308263, 9.767571684737765249E-15, 112.9440587442963562 ) ) ;
#13235 = FACE_OUTER_BOUND ( 'NONE', #6964, .T. ) ;
#13236 = LINE ( 'NONE', #9988, #8747 ) ;
#13237 = ORIENTED_EDGE ( 'NONE', *, *, #3247, .T. ) ;
#13238 = EDGE_CURVE ( 'NONE', #1945, #8191, #13324, .T. ) ;
#13239 = CARTESIAN_POINT ( 'NONE',  ( 107.5000000000000000, 1.734524432274993541E-14, 40.00000000000000000 ) ) ;
#13240 = CARTESIAN_POINT ( 'NONE',  ( 0.000000000000000000, 0.000000000000000000, 248.9926560891072143 ) ) ;
#13241 = ADVANCED_FACE ( 'NONE', ( #18514 ), #7559, .T. ) ;
#13242 = EDGE_LOOP ( 'NONE', ( #18460, #4036, #11509, #16964, #8220 ) ) ;
#13243 = CARTESIAN_POINT ( 'NONE',  ( 144.1955966362266679, 102.2982297021113141, 39.99999999999999289 ) ) ;
#13244 = DIRECTION ( 'NONE',  ( -0.3747554100459959403, -0.9271237148521535021, 0.000000000000000000 ) ) ;
#13245 = DIRECTION ( 'NONE',  ( 1.000000000000000000, 0.000000000000000000, 0.000000000000000000 ) ) ;
#13246 = DIRECTION ( 'NONE',  ( -0.6718750000000006661, 0.7406645559057077888, -6.938893903907224433E-16 ) ) ;
#13247 = VECTOR ( 'NONE', #13117, 1000.000000000000000 ) ;
#13248 = CARTESIAN_POINT ( 'NONE',  ( 7.350000000000000533, 10.39230484541327471, 0.000000000000000000 ) ) ;
#13249 = CARTESIAN_POINT ( 'NONE',  ( 55.16472960512370349, -30.25670013172234363, 248.9926560891072143 ) ) ;
#13250 = EDGE_LOOP ( 'NONE', ( #4914, #10952, #8654, #19005 ) ) ;
#13251 = VECTOR ( 'NONE', #19930, 1000.000000000000000 ) ;
#13252 = EDGE_CURVE ( 'NONE', #9705, #4517, #1432, .T. ) ;
#13253 = CARTESIAN_POINT ( 'NONE',  ( -109.9999999999983515, 265.0000000000000000, 85.00000000000001421 ) ) ;
#13254 = VERTEX_POINT ( 'NONE', #7357 ) ;
#13255 = VERTEX_POINT ( 'NONE', #2664 ) ;
#13256 = DIRECTION ( 'NONE',  ( 0.3747554100459959958, 0.9271237148521535021, 0.000000000000000000 ) ) ;
#13257 = ORIENTED_EDGE ( 'NONE', *, *, #3793, .F. ) ;
#13258 = AXIS2_PLACEMENT_3D ( 'NONE', #16141, #2130, #8354 ) ;
#13259 = DIRECTION ( 'NONE',  ( 0.4999999999999979461, 0.8660254037844397068, 0.000000000000000000 ) ) ;
#13260 = VECTOR ( 'NONE', #11424, 1000.000000000000000 ) ;
#13261 = DIRECTION ( 'NONE',  ( 0.000000000000000000, 0.000000000000000000, 1.000000000000000000 ) ) ;
#13262 = ADVANCED_FACE ( 'NONE', ( #13586 ), #13899, .T. ) ;
#13263 = DIRECTION ( 'NONE',  ( -0.000000000000000000, -1.000000000000000000, -0.000000000000000000 ) ) ;
#13264 = DIRECTION ( 'NONE',  ( -0.000000000000000000, -0.000000000000000000, 1.000000000000000000 ) ) ;
#13265 = EDGE_CURVE ( 'NONE', #2533, #17037, #300, .T. ) ;
#13266 = ORIENTED_EDGE ( 'NONE', *, *, #16121, .F. ) ;
#13267 = AXIS2_PLACEMENT_3D ( 'NONE', #15766, #14435, #17615 ) ;
#13268 = CARTESIAN_POINT ( 'NONE',  ( -176.1792632384392050, -186.5724904703759535, 30.00000000000000000 ) ) ;
#13269 = DIRECTION ( 'NONE',  ( 1.000000000000000000, 0.000000000000000000, 0.000000000000000000 ) ) ;
#13270 = ADVANCED_FACE ( 'NONE', ( #3276 ), #4707, .T. ) ;
#13271 = CARTESIAN_POINT ( 'NONE',  ( 47.56244194535165093, 37.78198917157335757, 293.5832628385307999 ) ) ;
#13272 = LINE ( 'NONE', #5424, #7989 ) ;
#13273 = CARTESIAN_POINT ( 'NONE',  ( 56.50329132715945235, -22.30005961346246579, 293.5832628385307999 ) ) ;
#13274 = ADVANCED_FACE ( 'NONE', ( #3470 ), #14419, .T. ) ;
#13275 = CARTESIAN_POINT ( 'NONE',  ( -36.71940246244744799, 108.6254278180370250, 14.88498244535570869 ) ) ;
#13276 = DIRECTION ( 'NONE',  ( -1.000000000000000000, -1.047444401652940164E-14, 0.000000000000000000 ) ) ;
#13277 = CARTESIAN_POINT ( 'NONE',  ( 103.2967819461768073, 53.25886146954521649, 14.88498244535472992 ) ) ;
#13278 = VERTEX_POINT ( 'NONE', #12672 ) ;
#13279 = CARTESIAN_POINT ( 'NONE',  ( 60.68773558783009747, -2.629322876227576433, 293.5832628385307999 ) ) ;
#13280 = CARTESIAN_POINT ( 'NONE',  ( 56.50138340076689047, -22.29928840491054132, 283.5832628385307999 ) ) ;
#13281 = VERTEX_POINT ( 'NONE', #15750 ) ;
#13282 = VERTEX_POINT ( 'NONE', #9704 ) ;
#13283 =( BOUNDED_CURVE ( )  B_SPLINE_CURVE ( 3, ( #14959, #15265, #15370, #10349 ),
 .UNSPECIFIED., .F., .F. ) 
 B_SPLINE_CURVE_WITH_KNOTS ( ( 4, 4 ),
 ( 1.570796326794896558, 3.141592653589793116 ),
 .UNSPECIFIED. ) 
 CURVE ( )  GEOMETRIC_REPRESENTATION_ITEM ( )  RATIONAL_B_SPLINE_CURVE ( ( 1.000000000000000000, 0.8047378541243649375, 0.8047378541243649375, 1.000000000000000000 ) ) 
 REPRESENTATION_ITEM ( '' )  );
#13284 = AXIS2_PLACEMENT_3D ( 'NONE', #17205, #4720, #11050 ) ;
#13285 = VERTEX_POINT ( 'NONE', #12461 ) ;
#13286 = DIRECTION ( 'NONE',  ( 0.8479630283625716469, -0.5300553768524345344, 0.000000000000000000 ) ) ;
#13287 = CARTESIAN_POINT ( 'NONE',  ( -148.9554720520392834, -17.67108784863415138, 60.00000000000000000 ) ) ;
#13288 = ORIENTED_EDGE ( 'NONE', *, *, #17969, .F. ) ;
#13289 = CARTESIAN_POINT ( 'NONE',  ( 95.44915936928622102, -116.0550301922294665, 7.385628739980171886 ) ) ;
#13290 = CARTESIAN_POINT ( 'NONE',  ( -82.65886493343872132, -125.1699850288409408, 4.855373681067642444 ) ) ;
#13291 = CIRCLE ( 'NONE', #3520, 62.91752772691707207 ) ;
#13292 = LINE ( 'NONE', #5641, #19298 ) ;
#13293 = CYLINDRICAL_SURFACE ( 'NONE', #4964, 150.0000000000000284 ) ;
#13294 = PLANE ( 'NONE',  #2416 ) ;
#13295 = VECTOR ( 'NONE', #7445, 1000.000000000000000 ) ;
#13296 = DIRECTION ( 'NONE',  ( 0.000000000000000000, 0.000000000000000000, 1.000000000000000000 ) ) ;
#13297 = VECTOR ( 'NONE', #2702, 1000.000000000000000 ) ;
#13298 = CARTESIAN_POINT ( 'NONE',  ( 113.3640620605769413, -25.59923667990641150, 14.88498244535466064 ) ) ;
#13299 = CARTESIAN_POINT ( 'NONE',  ( 1.396592535537252080E-14, 0.000000000000000000, 127.7817459305202448 ) ) ;
#13300 = DIRECTION ( 'NONE',  ( 6.982962677686266711E-15, 0.000000000000000000, 1.000000000000000000 ) ) ;
#13301 = ORIENTED_EDGE ( 'NONE', *, *, #1147, .F. ) ;
#13302 = DIRECTION ( 'NONE',  ( -0.1736481776669172583, -0.9848077530122103518, 0.000000000000000000 ) ) ;
#13303 = DIRECTION ( 'NONE',  ( 0.5000000000000039968, 0.8660254037844362651, -3.488064225688950243E-15 ) ) ;
#13304 = ORIENTED_EDGE ( 'NONE', *, *, #11613, .F. ) ;
#13305 =( NAMED_UNIT ( * ) SI_UNIT ( $, .STERADIAN. ) SOLID_ANGLE_UNIT ( ) );
#13306 = AXIS2_PLACEMENT_3D ( 'NONE', #6506, #11298, #3428 ) ;
#13307 = VERTEX_POINT ( 'NONE', #12774 ) ;
#13308 = AXIS2_PLACEMENT_3D ( 'NONE', #19096, #935, #5551 ) ;
#13309 = CARTESIAN_POINT ( 'NONE',  ( -176.7850001792984926, -190.0000000000000284, 6.572490470375933036 ) ) ;
#13310 = ORIENTED_EDGE ( 'NONE', *, *, #16128, .T. ) ;
#13311 = CARTESIAN_POINT ( 'NONE',  ( 45.48770046196260353, 37.09555676057011908, 132.4711112102474146 ) ) ;
#13312 = PLANE ( 'NONE',  #8941 ) ;
#13313 = CARTESIAN_POINT ( 'NONE',  ( -2.300765332208364988, -116.0870680293436408, 14.88498244535546711 ) ) ;
#13314 = DIRECTION ( 'NONE',  ( 0.000000000000000000, 0.000000000000000000, 1.000000000000000000 ) ) ;
#13315 = FACE_OUTER_BOUND ( 'NONE', #20122, .T. ) ;
#13316 = ADVANCED_FACE ( 'NONE', ( #14211 ), #4875, .F. ) ;
#13317 = ORIENTED_EDGE ( 'NONE', *, *, #16292, .T. ) ;
#13318 = CARTESIAN_POINT ( 'NONE',  ( -1.289614712049164114, 5.590028426173843101, 283.5832628385307999 ) ) ;
#13319 = CARTESIAN_POINT ( 'NONE',  ( -132.0570769712681169, -87.76803911442084427, 0.2774143636855481709 ) ) ;
#13320 = FACE_OUTER_BOUND ( 'NONE', #16667, .T. ) ;
#13321 = VECTOR ( 'NONE', #19521, 1000.000000000000000 ) ;
#13322 = DIRECTION ( 'NONE',  ( -0.000000000000000000, -0.000000000000000000, 1.000000000000000000 ) ) ;
#13323 = CARTESIAN_POINT ( 'NONE',  ( 113.5802308907677372, 8.308367629983374414, 39.88498244535465886 ) ) ;
#13324 = CIRCLE ( 'NONE', #610, 7.500000000000002665 ) ;
#13325 = CARTESIAN_POINT ( 'NONE',  ( -132.7096788433825907, -70.03826381905778931, 34.33854327515700788 ) ) ;
#13326 = AXIS2_PLACEMENT_3D ( 'NONE', #14429, #18664, #10865 ) ;
#13327 = ORIENTED_EDGE ( 'NONE', *, *, #220, .F. ) ;
#13328 = VECTOR ( 'NONE', #9628, 999.9999999999998863 ) ;
#13329 = VERTEX_POINT ( 'NONE', #1531 ) ;
#13330 = EDGE_CURVE ( 'NONE', #13976, #3773, #17608, .T. ) ;
#13331 = ORIENTED_EDGE ( 'NONE', *, *, #5173, .T. ) ;
#13332 = ORIENTED_EDGE ( 'NONE', *, *, #772, .T. ) ;
#13333 = EDGE_CURVE ( 'NONE', #16627, #7331, #1944, .T. ) ;
#13334 = VERTEX_POINT ( 'NONE', #9607 ) ;
#13335 = AXIS2_PLACEMENT_3D ( 'NONE', #7420, #7225, #7520 ) ;
#13336 = AXIS2_PLACEMENT_3D ( 'NONE', #4147, #11711, #18165 ) ;
#13337 = DIRECTION ( 'NONE',  ( 1.000000000000000000, 0.000000000000000000, -6.994638739193269649E-15 ) ) ;
#13338 = VECTOR ( 'NONE', #4769, 1000.000000000000114 ) ;
#13339 = CARTESIAN_POINT ( 'NONE',  ( -57.65577537092151772, 11.00103590902930328, 132.4711112102474146 ) ) ;
#13340 = CARTESIAN_POINT ( 'NONE',  ( 7.500000000000001776, 60.00000000000000000, -105.0000000000000142 ) ) ;
#13341 = ORIENTED_EDGE ( 'NONE', *, *, #5007, .F. ) ;
#13342 = DIRECTION ( 'NONE',  ( -1.000000000000000000, 0.000000000000000000, 6.969309079188926949E-15 ) ) ;
#13343 = DIRECTION ( 'NONE',  ( 0.000000000000000000, 0.000000000000000000, 1.000000000000000000 ) ) ;
#13344 = ADVANCED_FACE ( 'NONE', ( #11238 ), #6651, .T. ) ;
#13345 = EDGE_LOOP ( 'NONE', ( #1910, #5688, #1853, #14078 ) ) ;
#13346 = FACE_OUTER_BOUND ( 'NONE', #19583, .T. ) ;
#13347 = FACE_OUTER_BOUND ( 'NONE', #2740, .T. ) ;
#13348 = CYLINDRICAL_SURFACE ( 'NONE', #12371, 150.0000000000000284 ) ;
#13349 = DIRECTION ( 'NONE',  ( 0.000000000000000000, 1.000000000000000000, 0.000000000000000000 ) ) ;
#13350 = VECTOR ( 'NONE', #15999, 1000.000000000000000 ) ;
#13351 = DIRECTION ( 'NONE',  ( -0.9993852124581887875, 0.03505990758545896036, 0.000000000000000000 ) ) ;
#13352 = CARTESIAN_POINT ( 'NONE',  ( -189.9999999999988916, 285.0000000000000568, 5.000000000000268230 ) ) ;
#13353 = VECTOR ( 'NONE', #19293, 1000.000000000000000 ) ;
#13354 = VECTOR ( 'NONE', #7200, 999.9999999999998863 ) ;
#13355 = EDGE_LOOP ( 'NONE', ( #18778, #3763, #3947 ) ) ;
#13356 = EDGE_CURVE ( 'NONE', #9378, #4265, #3173, .T. ) ;
#13357 = DIRECTION ( 'NONE',  ( -6.982962677686266711E-15, 0.000000000000000000, -1.000000000000000000 ) ) ;
#13358 = VERTEX_POINT ( 'NONE', #17496 ) ;
#13359 = EDGE_CURVE ( 'NONE', #2297, #19640, #11391, .T. ) ;
#13360 = ORIENTED_EDGE ( 'NONE', *, *, #370, .F. ) ;
#13361 = CARTESIAN_POINT ( 'NONE',  ( -110.0000000000000142, 275.0000000000000568, 39.99999999999997868 ) ) ;
#13362 = EDGE_LOOP ( 'NONE', ( #101, #12001, #19311, #10464 ) ) ;
#13363 = ORIENTED_EDGE ( 'NONE', *, *, #18257, .F. ) ;
#13364 = DIRECTION ( 'NONE',  ( -0.1736481776669206722, -0.9848077530122097967, 0.000000000000000000 ) ) ;
#13365 = FACE_OUTER_BOUND ( 'NONE', #15518, .T. ) ;
#13366 = LINE ( 'NONE', #2647, #1488 ) ;
#13367 = DIRECTION ( 'NONE',  ( 1.000000000000000000, 0.000000000000000000, 0.000000000000000000 ) ) ;
#13368 = AXIS2_PLACEMENT_3D ( 'NONE', #18726, #3074, #12265 ) ;
#13369 = CIRCLE ( 'NONE', #4568, 106.4288957539801146 ) ;
#13370 = ORIENTED_EDGE ( 'NONE', *, *, #12205, .F. ) ;
#13371 = EDGE_CURVE ( 'NONE', #14025, #18229, #15656, .T. ) ;
#13372 = CARTESIAN_POINT ( 'NONE',  ( -135.0159133995099126, -65.35183200177806384, 32.89269165050915689 ) ) ;
#13373 = CARTESIAN_POINT ( 'NONE',  ( 0.000000000000000000, 0.000000000000000000, 248.9926560891072143 ) ) ;
#13374 = FACE_OUTER_BOUND ( 'NONE', #2614, .T. ) ;
#13375 = DIRECTION ( 'NONE',  ( -0.9396926207859114255, 0.3420201433256601642, 0.000000000000000000 ) ) ;
#13376 = ORIENTED_EDGE ( 'NONE', *, *, #16410, .F. ) ;
#13377 = DIRECTION ( 'NONE',  ( -1.613511099790691498E-16, 1.000000000000000000, -0.000000000000000000 ) ) ;
#13378 = CARTESIAN_POINT ( 'NONE',  ( 0.000000000000000000, 0.000000000000000000, 293.5832628385307999 ) ) ;
#13379 = CARTESIAN_POINT ( 'NONE',  ( -150.0000000000000284, 0.000000000000000000, 49.99999999999999289 ) ) ;
#13380 = ORIENTED_EDGE ( 'NONE', *, *, #10844, .F. ) ;
#13381 = AXIS2_PLACEMENT_3D ( 'NONE', #7348, #13790, #12147 ) ;
#13382 = CARTESIAN_POINT ( 'NONE',  ( 0.000000000000000000, 0.000000000000000000, 132.4711112102474146 ) ) ;
#13383 = FACE_OUTER_BOUND ( 'NONE', #19430, .T. ) ;
#13384 = AXIS2_PLACEMENT_3D ( 'NONE', #17106, #7684, #9116 ) ;
#13385 = EDGE_CURVE ( 'NONE', #15515, #13023, #1834, .T. ) ;
#13386 = ORIENTED_EDGE ( 'NONE', *, *, #9651, .T. ) ;
#13387 = ADVANCED_FACE ( 'NONE', ( #96 ), #3072, .F. ) ;
#13388 = ORIENTED_EDGE ( 'NONE', *, *, #13792, .F. ) ;
#13389 = ORIENTED_EDGE ( 'NONE', *, *, #17283, .F. ) ;
#13390 = CARTESIAN_POINT ( 'NONE',  ( -133.2435246741110006, -68.89240257401093004, 30.00000000000000000 ) ) ;
#13391 = LINE ( 'NONE', #18210, #10997 ) ;
#13392 = ORIENTED_EDGE ( 'NONE', *, *, #17400, .T. ) ;
#13393 = CARTESIAN_POINT ( 'NONE',  ( 103.0319911124603323, -126.0382377111977092, 1.048486719239181131 ) ) ;
#13394 = CARTESIAN_POINT ( 'NONE',  ( -104.7095274995498357, -123.3473593051618451, 0.3789873141021475322 ) ) ;
#13395 = EDGE_CURVE ( 'NONE', #18230, #4188, #8066, .T. ) ;
#13396 = VECTOR ( 'NONE', #11148, 999.9999999999998863 ) ;
#13397 = CARTESIAN_POINT ( 'NONE',  ( -58.69016442926521648, -1.379293853801960124, 112.7772637782949516 ) ) ;
#13398 = CARTESIAN_POINT ( 'NONE',  ( -30.53958573130872978, 50.13752642112859803, 132.4711112102474146 ) ) ;
#13399 = CARTESIAN_POINT ( 'NONE',  ( 128.2779226595531270, 102.2982297021113141, 39.99999999999999289 ) ) ;
#13400 =( LENGTH_UNIT ( ) NAMED_UNIT ( * ) SI_UNIT ( .MILLI., .METRE. ) );
#13401 = CARTESIAN_POINT ( 'NONE',  ( 45.46865632508072963, -40.28046525994365368, 293.5832628385307999 ) ) ;
#13402 = DIRECTION ( 'NONE',  ( -0.000000000000000000, -0.000000000000000000, 1.000000000000000000 ) ) ;
#13403 = ORIENTED_EDGE ( 'NONE', *, *, #12594, .T. ) ;
#13404 = CARTESIAN_POINT ( 'NONE',  ( -109.9999999999983515, 275.0000000000000000, 85.00000000000001421 ) ) ;
#13405 = CARTESIAN_POINT ( 'NONE',  ( 0.000000000000000000, 0.000000000000000000, 248.9926560891072143 ) ) ;
#13406 = EDGE_CURVE ( 'NONE', #6975, #9578, #6347, .T. ) ;
#13407 = ORIENTED_EDGE ( 'NONE', *, *, #5928, .T. ) ;
#13408 = VECTOR ( 'NONE', #490, 1000.000000000000000 ) ;
#13409 = ORIENTED_EDGE ( 'NONE', *, *, #4389, .T. ) ;
#13410 = VERTEX_POINT ( 'NONE', #6451 ) ;
#13411 = ADVANCED_FACE ( 'NONE', ( #11138 ), #17396, .F. ) ;
#13412 = DIRECTION ( 'NONE',  ( -0.000000000000000000, -0.000000000000000000, 1.000000000000000000 ) ) ;
#13413 = VERTEX_POINT ( 'NONE', #17992 ) ;
#13414 = LINE ( 'NONE', #19665, #13821 ) ;
#13415 = CARTESIAN_POINT ( 'NONE',  ( -38.41834839689332171, 68.18670162478844077, 110.9660488491356887 ) ) ;
#13416 = CARTESIAN_POINT ( 'NONE',  ( -56.84754764479025368, -154.7316448359455308, 60.00000000000000000 ) ) ;
#13417 = DIRECTION ( 'NONE',  ( 0.000000000000000000, 0.000000000000000000, 1.000000000000000000 ) ) ;
#13418 = ORIENTED_EDGE ( 'NONE', *, *, #10006, .T. ) ;
#13419 = CARTESIAN_POINT ( 'NONE',  ( 45.48770046196260353, 37.09555676057011908, 110.7293897666001214 ) ) ;
#13420 = FACE_OUTER_BOUND ( 'NONE', #15018, .T. ) ;
#13421 = VECTOR ( 'NONE', #5844, 1000.000000000000000 ) ;
#13422 = PLANE ( 'NONE',  #4310 ) ;
#13423 = DIRECTION ( 'NONE',  ( 1.000000000000000000, 0.000000000000000000, 0.000000000000000000 ) ) ;
#13424 = PRODUCT_DEFINITION_FORMATION_WITH_SPECIFIED_SOURCE ( 'ANY', '', #1811, .NOT_KNOWN. ) ;
#13425 = DIRECTION ( 'NONE',  ( 1.000000000000000000, 0.000000000000000000, 0.000000000000000000 ) ) ;
#13426 = CARTESIAN_POINT ( 'NONE',  ( 57.61627707419552280, 19.23614321207256239, 293.5832628385307999 ) ) ;
#13427 = ORIENTED_EDGE ( 'NONE', *, *, #4068, .F. ) ;
#13428 = EDGE_LOOP ( 'NONE', ( #18455, #12820, #17221, #3931 ) ) ;
#13429 = ORIENTED_EDGE ( 'NONE', *, *, #13876, .F. ) ;
#13430 = VERTEX_POINT ( 'NONE', #6844 ) ;
#13431 = EDGE_CURVE ( 'NONE', #19763, #2611, #597, .T. ) ;
#13432 = ORIENTED_EDGE ( 'NONE', *, *, #12258, .F. ) ;
#13433 = CARTESIAN_POINT ( 'NONE',  ( 107.5000000000000000, -118.5063289449133350, -10.00000000000000355 ) ) ;
#13434 = LINE ( 'NONE', #4341, #13189 ) ;
#13435 = CARTESIAN_POINT ( 'NONE',  ( -30.25670013172252837, -55.16472960512360402, 248.9926560891072143 ) ) ;
#13436 = ORIENTED_EDGE ( 'NONE', *, *, #10721, .F. ) ;
#13437 = VECTOR ( 'NONE', #235, 1000.000000000000000 ) ;
#13438 = DIRECTION ( 'NONE',  ( 1.613511099790691498E-16, -1.000000000000000000, 0.000000000000000000 ) ) ;
#13439 = DIRECTION ( 'NONE',  ( 1.000000000000000000, 0.000000000000000000, 0.000000000000000000 ) ) ;
#13440 = ORIENTED_EDGE ( 'NONE', *, *, #16547, .F. ) ;
#13441 = DIRECTION ( 'NONE',  ( 1.000000000000000000, 0.000000000000000000, 0.000000000000000000 ) ) ;
#13442 = EDGE_CURVE ( 'NONE', #17764, #6419, #6971, .T. ) ;
#13443 = DIRECTION ( 'NONE',  ( -0.7660444431189835646, 0.6427876096865328126, -0.000000000000000000 ) ) ;
#13444 = CARTESIAN_POINT ( 'NONE',  ( 148.9554720520395392, -17.67108784863215476, 60.00000000000000000 ) ) ;
#13445 = CARTESIAN_POINT ( 'NONE',  ( 0.000000000000000000, 0.000000000000000000, 0.000000000000000000 ) ) ;
#13446 = DIRECTION ( 'NONE',  ( -0.1736481776669374366, 0.9848077530122066880, 0.000000000000000000 ) ) ;
#13447 = CARTESIAN_POINT ( 'NONE',  ( 60.72279549541555355, -1.629937663769388090, 293.5832628385307999 ) ) ;
#13448 = ORIENTED_EDGE ( 'NONE', *, *, #19988, .F. ) ;
#13449 = CARTESIAN_POINT ( 'NONE',  ( 0.000000000000000000, 0.000000000000000000, 283.5832628385307999 ) ) ;
#13450 = VECTOR ( 'NONE', #13109, 1000.000000000000000 ) ;
#13451 = AXIS2_PLACEMENT_3D ( 'NONE', #10741, #15454, #18220 ) ;
#13452 = EDGE_LOOP ( 'NONE', ( #16085, #10297, #3540, #14003, #8453 ) ) ;
#13453 = VERTEX_POINT ( 'NONE', #3961 ) ;
#13454 = ADVANCED_FACE ( 'NONE', ( #2438 ), #11542, .T. ) ;
#13455 = DIRECTION ( 'NONE',  ( -0.3427509529624095941, -0.9394263059140722794, 0.000000000000000000 ) ) ;
#13456 = EDGE_CURVE ( 'NONE', #10750, #12303, #2044, .T. ) ;
#13457 = ORIENTED_EDGE ( 'NONE', *, *, #10355, .T. ) ;
#13458 = EDGE_LOOP ( 'NONE', ( #8092, #4321, #15438, #19152, #11467, #5383 ) ) ;
#13459 = AXIS2_PLACEMENT_3D ( 'NONE', #15027, #7255, #13477 ) ;
#13460 = FACE_OUTER_BOUND ( 'NONE', #13766, .T. ) ;
#13461 = CARTESIAN_POINT ( 'NONE',  ( -95.40880945838063099, -115.7543288757354389, 49.20016699389176296 ) ) ;
#13462 = DIRECTION ( 'NONE',  ( 1.000000000000000000, 0.000000000000000000, -6.977185866873308817E-15 ) ) ;
#13463 = DIRECTION ( 'NONE',  ( 0.5000000000000009992, -0.8660254037844380415, 0.000000000000000000 ) ) ;
#13464 = ORIENTED_EDGE ( 'NONE', *, *, #17033, .F. ) ;
#13465 = EDGE_CURVE ( 'NONE', #1941, #541, #4344, .T. ) ;
#13466 = CARTESIAN_POINT ( 'NONE',  ( -122.8001410695374460, -86.14014948502065749, 49.99999999999999289 ) ) ;
#13468 = CIRCLE ( 'NONE', #7595, 150.0000000000000284 ) ;
#13467 = CARTESIAN_POINT ( 'NONE',  ( 0.000000000000000000, 0.000000000000000000, 283.5832628385307999 ) ) ;
#13469 = AXIS2_PLACEMENT_3D ( 'NONE', #3553, #11009, #6531 ) ;
#13470 = EDGE_CURVE ( 'NONE', #10598, #10243, #13159, .T. ) ;
#13471 = DIRECTION ( 'NONE',  ( 0.000000000000000000, 0.000000000000000000, -1.000000000000000000 ) ) ;
#13472 = EDGE_CURVE ( 'NONE', #18388, #5457, #14615, .T. ) ;
#13473 = CARTESIAN_POINT ( 'NONE',  ( -54.67896814532655725, -21.36933070621745046, 111.4180192758973931 ) ) ;
#13474 = LINE ( 'NONE', #11935, #14305 ) ;
#13475 = AXIS2_PLACEMENT_3D ( 'NONE', #8669, #6747, #13162 ) ;
#13476 = PLANE ( 'NONE',  #9489 ) ;
#13477 = DIRECTION ( 'NONE',  ( 1.000000000000000000, 0.000000000000000000, 0.000000000000000000 ) ) ;
#13478 = VERTEX_POINT ( 'NONE', #12969 ) ;
#13479 = DIRECTION ( 'NONE',  ( -0.000000000000000000, -0.000000000000000000, 1.000000000000000000 ) ) ;
#13480 = DIRECTION ( 'NONE',  ( 1.000000000000000000, 0.000000000000000000, 0.000000000000000000 ) ) ;
#13481 = ORIENTED_EDGE ( 'NONE', *, *, #1328, .T. ) ;
#13482 = ORIENTED_EDGE ( 'NONE', *, *, #1472, .F. ) ;
#13483 = ADVANCED_FACE ( 'NONE', ( #14810 ), #10200, .F. ) ;
#13484 = CARTESIAN_POINT ( 'NONE',  ( -97.38440206417406841, -115.5262529913582341, 29.75236954509034248 ) ) ;
#13485 = EDGE_CURVE ( 'NONE', #13542, #10934, #18407, .T. ) ;
#13486 = VECTOR ( 'NONE', #8791, 1000.000000000000000 ) ;
#13487 = CYLINDRICAL_SURFACE ( 'NONE', #19585, 3.224098631618460331 ) ;
#13488 = LINE ( 'NONE', #6969, #19181 ) ;
#13489 = ORIENTED_EDGE ( 'NONE', *, *, #731, .F. ) ;
#13490 = AXIS2_PLACEMENT_3D ( 'NONE', #769, #7017, #5480 ) ;
#13491 = CARTESIAN_POINT ( 'NONE',  ( 0.000000000000000000, 0.000000000000000000, 283.5832628385307999 ) ) ;
#13492 = CARTESIAN_POINT ( 'NONE',  ( -98.69108797088911444, -112.9688971639520219, -9.907602633159209304 ) ) ;
#13493 = STYLED_ITEM ( 'NONE', ( #12650 ), #1186 ) ;
#13494 = EDGE_CURVE ( 'NONE', #6700, #7117, #6942, .T. ) ;
#13495 = ADVANCED_FACE ( 'NONE', ( #19429 ), #2243, .T. ) ;
#13496 = ADVANCED_FACE ( 'NONE', ( #16061 ), #5217, .T. ) ;
#13497 = DIRECTION ( 'NONE',  ( 0.000000000000000000, 1.000000000000000000, 0.000000000000000000 ) ) ;
#13498 = PLANE ( 'NONE',  #151 ) ;
#13499 = LINE ( 'NONE', #19750, #744 ) ;
#13500 = DIRECTION ( 'NONE',  ( 1.000000000000000000, 0.000000000000000000, 0.000000000000000000 ) ) ;
#13501 = CARTESIAN_POINT ( 'NONE',  ( -109.5721339228237667, 31.03941509555038181, 14.88498244535621851 ) ) ;
#13502 = CARTESIAN_POINT ( 'NONE',  ( 0.000000000000000000, 7.347880794884121708E-16, -6.000000000000001776 ) ) ;
#13503 = VERTEX_POINT ( 'NONE', #17701 ) ;
#13504 = LINE ( 'NONE', #741, #6144 ) ;
#13505 = CARTESIAN_POINT ( 'NONE',  ( -37.09555676056967144, 45.48770046196298011, 248.9926560891072143 ) ) ;
#13506 = ORIENTED_EDGE ( 'NONE', *, *, #5390, .T. ) ;
#13507 = CIRCLE ( 'NONE', #460, 3.224098631618453670 ) ;
#13508 = EDGE_LOOP ( 'NONE', ( #3049, #3469, #17114, #10440, #3883 ) ) ;
#13509 = ADVANCED_FACE ( 'NONE', ( #699 ), #5409, .T. ) ;
#13510 =( LENGTH_UNIT ( ) NAMED_UNIT ( * ) SI_UNIT ( .MILLI., .METRE. ) );
#13511 = VECTOR ( 'NONE', #12212, 1000.000000000000000 ) ;
#13512 = ORIENTED_EDGE ( 'NONE', *, *, #9001, .F. ) ;
#13513 = CARTESIAN_POINT ( 'NONE',  ( 42.50000000000000000, 0.000000000000000000, -100.0000000000000000 ) ) ;
#13514 = ORIENTED_EDGE ( 'NONE', *, *, #15502, .F. ) ;
#13515 = CARTESIAN_POINT ( 'NONE',  ( 134.4452567384424242, -75.00213249385288350, 5.696041659366085419 ) ) ;
#13516 = LINE ( 'NONE', #19768, #15391 ) ;
#13517 = DIRECTION ( 'NONE',  ( -0.000000000000000000, -0.000000000000000000, 1.000000000000000000 ) ) ;
#13518 = EDGE_CURVE ( 'NONE', #16088, #11620, #16355, .T. ) ;
#13519 = EDGE_CURVE ( 'NONE', #9109, #17054, #1407, .T. ) ;
#13520 = CIRCLE ( 'NONE', #14202, 9.000000000000000000 ) ;
#13521 = CARTESIAN_POINT ( 'NONE',  ( 7.350000000000000533, 5.196152422706624030, -9.000000000000001776 ) ) ;
#13522 = LINE ( 'NONE', #1044, #13354 ) ;
#13523 = ORIENTED_EDGE ( 'NONE', *, *, #19604, .T. ) ;
#13524 = CARTESIAN_POINT ( 'NONE',  ( 0.000000000000000000, 164.0736214083062805, 39.99999999999999289 ) ) ;
#13525 = CARTESIAN_POINT ( 'NONE',  ( -128.4575182282473804, -77.52436737398411992, -0.4480010861637727104 ) ) ;
#13526 = CARTESIAN_POINT ( 'NONE',  ( 125.8775035253788843, -81.60755858752881409, -1.037139294228612618 ) ) ;
#13527 = AXIS2_PLACEMENT_3D ( 'NONE', #19478, #19968, #8720 ) ;
#13528 = CARTESIAN_POINT ( 'NONE',  ( -23.23469325536272478, -13.41455640552162443, 14.88498244535561454 ) ) ;
#13529 = CARTESIAN_POINT ( 'NONE',  ( -189.9999999999988916, 275.0000000000000000, 12.50000000000027178 ) ) ;
#13530 = CARTESIAN_POINT ( 'NONE',  ( 101.6421356237309652, -199.9999999999999716, 39.99999999999999289 ) ) ;
#13531 = EDGE_CURVE ( 'NONE', #371, #1941, #7142, .T. ) ;
#13532 = ORIENTED_EDGE ( 'NONE', *, *, #19369, .T. ) ;
#13533 = DIRECTION ( 'NONE',  ( -0.000000000000000000, -0.000000000000000000, 1.000000000000000000 ) ) ;
#13534 = VECTOR ( 'NONE', #6284, 1000.000000000000000 ) ;
#13535 = ORIENTED_EDGE ( 'NONE', *, *, #10648, .T. ) ;
#13536 = ORIENTED_EDGE ( 'NONE', *, *, #2578, .F. ) ;
#13537 = CIRCLE ( 'NONE', #4744, 17.50000000000000355 ) ;
#13538 = EDGE_LOOP ( 'NONE', ( #11760, #11566, #3197, #5048 ) ) ;
#13539 = ORIENTED_EDGE ( 'NONE', *, *, #3498, .T. ) ;
#13540 = FACE_BOUND ( 'NONE', #19099, .T. ) ;
#13541 = DIRECTION ( 'NONE',  ( 0.000000000000000000, 0.000000000000000000, 1.000000000000000000 ) ) ;
#13542 = VERTEX_POINT ( 'NONE', #7431 ) ;
#13544 = CARTESIAN_POINT ( 'NONE',  ( 77.31114765718493231, -12.23146955673620795, 132.4711112102474146 ) ) ;
#13543 = AXIS2_PLACEMENT_3D ( 'NONE', #103, #9312, #7771 ) ;
#13545 = CARTESIAN_POINT ( 'NONE',  ( -159.9599531637108782, -36.50981547337168109, 39.99999999999999289 ) ) ;
#13546 = ORIENTED_EDGE ( 'NONE', *, *, #884, .T. ) ;
#13547 = LINE ( 'NONE', #18167, #18595 ) ;
#13548 = CARTESIAN_POINT ( 'NONE',  ( -110.0000000000000142, 275.0000000000000000, -67.49999999999997158 ) ) ;
#13549 = CARTESIAN_POINT ( 'NONE',  ( -47.22802745636877120, -134.7565053399285091, 49.99999999999999289 ) ) ;
#13550 = AXIS2_PLACEMENT_3D ( 'NONE', #11179, #8314, #8418 ) ;
#13551 = DIRECTION ( 'NONE',  ( -0.000000000000000000, -0.000000000000000000, 1.000000000000000000 ) ) ;
#13552 = UNCERTAINTY_MEASURE_WITH_UNIT (LENGTH_MEASURE( 1.000000000000000082E-05 ), #4370, 'distance_accuracy_value', 'NONE');
#13553 = CARTESIAN_POINT ( 'NONE',  ( 129.0037046021668914, -76.61892870329793936, 40.13063405744939161 ) ) ;
#13554 = DIRECTION ( 'NONE',  ( -0.4338837391175643932, 0.9009688679024161484, 0.000000000000000000 ) ) ;
#13555 = ORIENTED_EDGE ( 'NONE', *, *, #18353, .F. ) ;
#13556 = CARTESIAN_POINT ( 'NONE',  ( -25.47058595421603044, -74.01264520835144367, 248.9926560891072143 ) ) ;
#13557 = ORIENTED_EDGE ( 'NONE', *, *, #7912, .F. ) ;
#13558 = VECTOR ( 'NONE', #13567, 1000.000000000000000 ) ;
#13559 = ORIENTED_EDGE ( 'NONE', *, *, #4483, .T. ) ;
#13560 = DIRECTION ( 'NONE',  ( -1.000000000000000000, 8.881784197001252323E-16, 0.000000000000000000 ) ) ;
#13561 = ORIENTED_EDGE ( 'NONE', *, *, #2609, .F. ) ;
#13562 = ORIENTED_EDGE ( 'NONE', *, *, #19533, .F. ) ;
#13563 = CYLINDRICAL_SURFACE ( 'NONE', #7791, 60.74260934110282051 ) ;
#13564 =( NAMED_UNIT ( * ) SI_UNIT ( $, .STERADIAN. ) SOLID_ANGLE_UNIT ( ) );
#13565 = CARTESIAN_POINT ( 'NONE',  ( 0.000000000000000000, 0.000000000000000000, 283.5832628385307999 ) ) ;
#13566 = EDGE_LOOP ( 'NONE', ( #15175, #1136, #7478, #17894 ) ) ;
#13567 = DIRECTION ( 'NONE',  ( 0.000000000000000000, 0.000000000000000000, 1.000000000000000000 ) ) ;
#13568 = CARTESIAN_POINT ( 'NONE',  ( -57.55901709132179178, -11.54977938102067547, 132.4711112102474146 ) ) ;
#13569 = AXIS2_PLACEMENT_3D ( 'NONE', #18283, #12021, #4259 ) ;
#13570 = ORIENTED_EDGE ( 'NONE', *, *, #12777, .F. ) ;
#13571 = DIRECTION ( 'NONE',  ( 0.000000000000000000, 0.000000000000000000, 1.000000000000000000 ) ) ;
#13572 = DIRECTION ( 'NONE',  ( -0.3088643371590125697, 0.9511061040868803440, 0.000000000000000000 ) ) ;
#13573 = EDGE_CURVE ( 'NONE', #6720, #17320, #9064, .T. ) ;
#13574 = VECTOR ( 'NONE', #6561, 1000.000000000000000 ) ;
#13575 = FACE_OUTER_BOUND ( 'NONE', #10005, .T. ) ;
#13576 = ORIENTED_EDGE ( 'NONE', *, *, #11477, .F. ) ;
#13577 = DIRECTION ( 'NONE',  ( 0.000000000000000000, 0.000000000000000000, 1.000000000000000000 ) ) ;
#13578 = CARTESIAN_POINT ( 'NONE',  ( 28.06584155524102187, -53.86996498385662591, 293.5832628385307999 ) ) ;
#13579 = FACE_OUTER_BOUND ( 'NONE', #9148, .T. ) ;
#13580 = ORIENTED_EDGE ( 'NONE', *, *, #5175, .F. ) ;
#13581 = CARTESIAN_POINT ( 'NONE',  ( -41.48948842197086151, 47.29944656917798795, 132.4711112102474146 ) ) ;
#13582 = FACE_OUTER_BOUND ( 'NONE', #15778, .T. ) ;
#13583 = ORIENTED_EDGE ( 'NONE', *, *, #18132, .F. ) ;
#13584 = AXIS2_PLACEMENT_3D ( 'NONE', #11784, #19670, #17658 ) ;
#13585 = VERTEX_POINT ( 'NONE', #4061 ) ;
#13586 = FACE_OUTER_BOUND ( 'NONE', #12434, .T. ) ;
#13587 = VECTOR ( 'NONE', #477, 1000.000000000000000 ) ;
#13588 = ADVANCED_FACE ( 'NONE', ( #5913 ), #5656, .T. ) ;
#13589 = ADVANCED_FACE ( 'NONE', ( #8765 ), #18387, .F. ) ;
#13590 = VERTEX_POINT ( 'NONE', #19809 ) ;
#13591 = EDGE_CURVE ( 'NONE', #6775, #4330, #10489, .T. ) ;
#13592 = CARTESIAN_POINT ( 'NONE',  ( 71.18887634719571622, -147.8252249328912740, 49.99999999999999289 ) ) ;
#13593 = CARTESIAN_POINT ( 'NONE',  ( -37.78198917157317993, 47.56244194535179304, 293.5832628385307999 ) ) ;
#13594 = ORIENTED_EDGE ( 'NONE', *, *, #11115, .T. ) ;
#13595 = CARTESIAN_POINT ( 'NONE',  ( 103.8658874391963707, -124.7161237612890687, 0.6789692764135434322 ) ) ;
#13596 = CARTESIAN_POINT ( 'NONE',  ( 15.91767397667354800, 164.0736214083062805, 60.00000000000000000 ) ) ;
#13597 = AXIS2_PLACEMENT_3D ( 'NONE', #14624, #12401, #1095 ) ;
#13598 = EDGE_CURVE ( 'NONE', #9705, #4730, #10392, .T. ) ;
#13599 = CARTESIAN_POINT ( 'NONE',  ( -42.50000000000000000, 5.204748896376250896E-15, -115.0000000000000000 ) ) ;
#13600 = FACE_OUTER_BOUND ( 'NONE', #13872, .T. ) ;
#13601 = CARTESIAN_POINT ( 'NONE',  ( 79.05640494598115708, -127.4758205975433043, 39.99999999999999289 ) ) ;
#13602 = AXIS2_PLACEMENT_3D ( 'NONE', #9540, #17329, #6377 ) ;
#13603 = DIRECTION ( 'NONE',  ( 0.000000000000000000, 0.000000000000000000, 1.000000000000000000 ) ) ;
#13604 = DIRECTION ( 'NONE',  ( 0.000000000000000000, 0.000000000000000000, 1.000000000000000000 ) ) ;
#13605 = DIRECTION ( 'NONE',  ( -0.000000000000000000, 0.000000000000000000, 1.000000000000000000 ) ) ;
#13606 = CARTESIAN_POINT ( 'NONE',  ( 107.5000000000000284, -189.9999999999999716, 40.00000000000000000 ) ) ;
#13607 = ORIENTED_EDGE ( 'NONE', *, *, #14972, .T. ) ;
#13608 = AXIS2_PLACEMENT_3D ( 'NONE', #1849, #8490, #6764 ) ;
#13609 = DIRECTION ( 'NONE',  ( -0.000000000000000000, -0.000000000000000000, 1.000000000000000000 ) ) ;
#13610 = DIRECTION ( 'NONE',  ( 1.000000000000000000, 0.000000000000000000, 0.000000000000000000 ) ) ;
#13611 = ORIENTED_EDGE ( 'NONE', *, *, #19057, .T. ) ;
#13612 = ORIENTED_EDGE ( 'NONE', *, *, #2417, .T. ) ;
#13613 =( NAMED_UNIT ( * ) SI_UNIT ( $, .STERADIAN. ) SOLID_ANGLE_UNIT ( ) );
#13614 = EDGE_CURVE ( 'NONE', #5836, #5572, #4365, .T. ) ;
#13615 = EDGE_CURVE ( 'NONE', #1562, #7965, #7602, .T. ) ;
#13616 = EDGE_CURVE ( 'NONE', #2847, #6649, #12234, .T. ) ;
#13617 = DIRECTION ( 'NONE',  ( 0.9749279121818226201, 0.2225209339563185562, 0.000000000000000000 ) ) ;
#13618 = ORIENTED_EDGE ( 'NONE', *, *, #535, .T. ) ;
#13619 = CARTESIAN_POINT ( 'NONE',  ( 59.30716253403183913, -13.12726406102058441, 283.5832628385307999 ) ) ;
#13620 = AXIS2_PLACEMENT_3D ( 'NONE', #16238, #19499, #19310 ) ;
#13621 = AXIS2_PLACEMENT_3D ( 'NONE', #6546, #9397, #7857 ) ;
#13622 = CARTESIAN_POINT ( 'NONE',  ( 163.5019688434126977, -20.99123081650019529, 39.99999999999999289 ) ) ;
#13623 = CIRCLE ( 'NONE', #2866, 10.00000000000000888 ) ;
#13624 = DIRECTION ( 'NONE',  ( 0.7818314824680220321, 0.6234898018587433643, 0.000000000000000000 ) ) ;
#13625 = DIRECTION ( 'NONE',  ( 1.000000000000000000, 0.000000000000000000, 0.000000000000000000 ) ) ;
#13626 = EDGE_LOOP ( 'NONE', ( #14725, #8585, #17093, #15869, #2741 ) ) ;
#13627 = DIRECTION ( 'NONE',  ( 1.000000000000000000, 0.000000000000000000, 0.000000000000000000 ) ) ;
#13628 = CARTESIAN_POINT ( 'NONE',  ( -132.8916714744451610, -69.69402298601710299, 6.374937744456566691 ) ) ;
#13629 = EDGE_CURVE ( 'NONE', #19407, #2612, #2534, .T. ) ;
#13630 = CARTESIAN_POINT ( 'NONE',  ( 130.6561114389107274, -73.68416578909177872, -5.683737997257604313 ) ) ;
#13631 = DIRECTION ( 'NONE',  ( 0.000000000000000000, 0.000000000000000000, -1.000000000000000000 ) ) ;
#13632 = FACE_OUTER_BOUND ( 'NONE', #12279, .T. ) ;
#13633 = CARTESIAN_POINT ( 'NONE',  ( -49.59485801383840453, -102.5175491340983882, 39.88498244535580284 ) ) ;
#13634 = ORIENTED_EDGE ( 'NONE', *, *, #16730, .F. ) ;
#13635 = LINE ( 'NONE', #19320, #2699 ) ;
#13636 = AXIS2_PLACEMENT_3D ( 'NONE', #6725, #3255, #482 ) ;
#13638 = ORIENTED_EDGE ( 'NONE', *, *, #3886, .F. ) ;
#13637 = AXIS2_PLACEMENT_3D ( 'NONE', #3857, #11720, #10192 ) ;
#13639 = EDGE_LOOP ( 'NONE', ( #5117, #364, #6217, #9307 ) ) ;
#13640 = EDGE_CURVE ( 'NONE', #2094, #6317, #12181, .T. ) ;
#13641 = EDGE_CURVE ( 'NONE', #3790, #10591, #11198, .T. ) ;
#13642 = EDGE_CURVE ( 'NONE', #10957, #16647, #17434, .T. ) ;
#13643 = EDGE_LOOP ( 'NONE', ( #1061, #12561, #11080, #15294 ) ) ;
#13644 = VERTEX_POINT ( 'NONE', #4163 ) ;
#13645 = ADVANCED_FACE ( 'NONE', ( #16652 ), #7533, .F. ) ;
#13646 = FACE_BOUND ( 'NONE', #7703, .T. ) ;
#13647 = DIRECTION ( 'NONE',  ( 1.000000000000000000, 0.000000000000000000, 0.000000000000000000 ) ) ;
#13648 = EDGE_LOOP ( 'NONE', ( #8534, #6920, #6412, #983 ) ) ;
#13649 = CARTESIAN_POINT ( 'NONE',  ( 77.50000000000000000, 0.000000000000000000, -105.0000000000000142 ) ) ;
#13650 = DIRECTION ( 'NONE',  ( -1.000000000000000000, -0.000000000000000000, -0.000000000000000000 ) ) ;
#13651 = VECTOR ( 'NONE', #15500, 1000.000000000000114 ) ;
#13652 = ORIENTED_EDGE ( 'NONE', *, *, #13759, .T. ) ;
#13653 = CARTESIAN_POINT ( 'NONE',  ( -88.33722569973700445, 105.0987966894255550, -22.54091672644404909 ) ) ;
#13654 = CONICAL_SURFACE ( 'NONE', #14332, 32.50000000000000000, 0.7853981633974510546 ) ;
#13655 = EDGE_CURVE ( 'NONE', #12459, #7604, #5984, .T. ) ;
#13656 = FACE_OUTER_BOUND ( 'NONE', #18290, .T. ) ;
#13657 = CARTESIAN_POINT ( 'NONE',  ( -132.8189972983174698, -84.37332251142817086, 0.9521473212757564086 ) ) ;
#13658 = CARTESIAN_POINT ( 'NONE',  ( -53.86996498385653354, -28.06584155524119950, 283.5832628385307999 ) ) ;
#13659 = CARTESIAN_POINT ( 'NONE',  ( 123.8648416762537039, -84.61253400034586036, 40.61864639473208172 ) ) ;
#13660 = CYLINDRICAL_SURFACE ( 'NONE', #10645, 10.00000000000000888 ) ;
#13661 = ORIENTED_EDGE ( 'NONE', *, *, #20144, .T. ) ;
#13662 = DIRECTION ( 'NONE',  ( 1.000000000000000000, 0.000000000000000000, 0.000000000000000000 ) ) ;
#13663 = VECTOR ( 'NONE', #13879, 1000.000000000000227 ) ;
#13664 = ORIENTED_EDGE ( 'NONE', *, *, #5833, .T. ) ;
#13665 = AXIS2_PLACEMENT_3D ( 'NONE', #11688, #5461, #17845 ) ;
#13666 = AXIS2_PLACEMENT_3D ( 'NONE', #19043, #11248, #5028 ) ;
#13667 = VERTEX_POINT ( 'NONE', #8864 ) ;
#13668 = CARTESIAN_POINT ( 'NONE',  ( 0.000000000000000000, 0.000000000000000000, 283.5832628385307999 ) ) ;
#13669 = AXIS2_PLACEMENT_3D ( 'NONE', #16115, #16018, #4877 ) ;
#13670 = ORIENTED_EDGE ( 'NONE', *, *, #8335, .F. ) ;
#13671 = DIRECTION ( 'NONE',  ( 0.000000000000000000, 0.000000000000000000, 1.000000000000000000 ) ) ;
#13672 = EDGE_CURVE ( 'NONE', #15515, #13875, #2389, .T. ) ;
#13673 = DIRECTION ( 'NONE',  ( 0.7818314824680220321, 0.6234898018587433643, 0.000000000000000000 ) ) ;
#13674 = FILL_AREA_STYLE ('',( #2948 ) ) ;
#13675 = CARTESIAN_POINT ( 'NONE',  ( 107.5000000000000284, -199.9999999999999716, 10.00000000000000178 ) ) ;
#13676 = EDGE_LOOP ( 'NONE', ( #15570, #8977, #1045, #15204, #11550 ) ) ;
#13677 = CYLINDRICAL_SURFACE ( 'NONE', #9348, 60.74260934110282051 ) ;
#13678 = DIRECTION ( 'NONE',  ( 0.000000000000000000, 1.000000000000000000, 0.000000000000000000 ) ) ;
#13679 = VERTEX_POINT ( 'NONE', #12027 ) ;
#13680 = DIRECTION ( 'NONE',  ( -0.000000000000000000, 0.000000000000000000, -1.000000000000000000 ) ) ;
#13681 = CARTESIAN_POINT ( 'NONE',  ( 0.000000000000000000, 0.000000000000000000, -105.0000000000000142 ) ) ;
#13682 = AXIS2_PLACEMENT_3D ( 'NONE', #14700, #689, #11434 ) ;
#13683 = LINE ( 'NONE', #4380, #14212 ) ;
#13684 = VERTEX_POINT ( 'NONE', #4262 ) ;
#13685 = CARTESIAN_POINT ( 'NONE',  ( 70.38703763562273252, -92.47916748300480094, 14.88498244535495907 ) ) ;
#13686 = DIRECTION ( 'NONE',  ( 0.000000000000000000, 0.000000000000000000, 1.000000000000000000 ) ) ;
#13687 = DIRECTION ( 'NONE',  ( 1.000000000000000000, 0.000000000000000000, 0.000000000000000000 ) ) ;
#13688 = ORIENTED_EDGE ( 'NONE', *, *, #2241, .T. ) ;
#13689 = FACE_OUTER_BOUND ( 'NONE', #8194, .T. ) ;
#13690 = CYLINDRICAL_SURFACE ( 'NONE', #7953, 39.99999999999997868 ) ;
#13691 = ORIENTED_EDGE ( 'NONE', *, *, #7366, .T. ) ;
#13692 = B_SPLINE_CURVE_WITH_KNOTS ( 'NONE', 3,
 ( #3751, #976, #7224, #7519, #3032, #4251 ),
 .UNSPECIFIED., .F., .F.,
 ( 4, 2, 4 ),
 ( 2.380730968223946593E-07, 0.002629065763328364801, 0.005257893453559907108 ),
 .UNSPECIFIED. ) ;
#13693 = ORIENTED_EDGE ( 'NONE', *, *, #398, .F. ) ;
#13694 = DIRECTION ( 'NONE',  ( -1.000000000000000000, 0.000000000000000000, 0.000000000000000000 ) ) ;
#13695 = VERTEX_POINT ( 'NONE', #15202 ) ;
#13696 = CIRCLE ( 'NONE', #2598, 110.0000000000000142 ) ;
#13697 = AXIS2_PLACEMENT_3D ( 'NONE', #3946, #18070, #12009 ) ;
#13698 = EDGE_CURVE ( 'NONE', #18902, #5832, #19913, .T. ) ;
#13699 = CARTESIAN_POINT ( 'NONE',  ( 53.87178215532755132, 28.06680738835045119, 293.5832628385307999 ) ) ;
#13700 = DIRECTION ( 'NONE',  ( 0.9396926207859126468, -0.3420201433256568890, 0.000000000000000000 ) ) ;
#13701 = VERTEX_POINT ( 'NONE', #16745 ) ;
#13702 = CARTESIAN_POINT ( 'NONE',  ( 82.23581699221259100, -125.4482974261017745, 7.029979419219573700 ) ) ;
#13703 = CYLINDRICAL_SURFACE ( 'NONE', #9959, 60.74260934110282051 ) ;
#13704 = CARTESIAN_POINT ( 'NONE',  ( -136.2020012053989433, -31.16171794781974214, -14.16315223586064498 ) ) ;
#13705 = CARTESIAN_POINT ( 'NONE',  ( 61.98599999999999000, 0.000000000000000000, 6.000000000000001776 ) ) ;
#13706 = FACE_BOUND ( 'NONE', #5192, .T. ) ;
#13707 = ADVANCED_FACE ( 'NONE', ( #2738 ), #19009, .T. ) ;
#13708 = FACE_BOUND ( 'NONE', #12085, .T. ) ;
#13709 = CARTESIAN_POINT ( 'NONE',  ( 45.84586732611860782, -36.66871011346395193, 110.7293897666001214 ) ) ;
#13710 = CARTESIAN_POINT ( 'NONE',  ( -22.81000261549328911, 58.63718168490508020, 293.5832628385307999 ) ) ;
#13711 = AXIS2_PLACEMENT_3D ( 'NONE', #5873, #12087, #10866 ) ;
#13712 = CARTESIAN_POINT ( 'NONE',  ( 95.72167172977059124, -116.1306513017061519, 30.88982041833051539 ) ) ;
#13713 = ORIENTED_EDGE ( 'NONE', *, *, #13598, .F. ) ;
#13714 = CARTESIAN_POINT ( 'NONE',  ( -8.938941455414985526, 60.08127757648384915, 283.5832628385307999 ) ) ;
#13715 = CARTESIAN_POINT ( 'NONE',  ( 0.000000000000000000, 0.000000000000000000, 248.9926560891072143 ) ) ;
#13716 = EDGE_LOOP ( 'NONE', ( #1296, #14338, #15247, #14833, #15332, #19816, #10812, #3825, #4711, #14112, #11422 ) ) ;
#13717 = EDGE_LOOP ( 'NONE', ( #12161, #10292, #15423, #66 ) ) ;
#13718 = ORIENTED_EDGE ( 'NONE', *, *, #9887, .T. ) ;
#13719 = ADVANCED_FACE ( 'NONE', ( #15724 ), #11006, .T. ) ;
#13720 = VECTOR ( 'NONE', #7858, 1000.000000000000000 ) ;
#13721 = FACE_BOUND ( 'NONE', #4063, .T. ) ;
#13722 = VERTEX_POINT ( 'NONE', #1505 ) ;
#13723 = VECTOR ( 'NONE', #9366, 1000.000000000000114 ) ;
#13724 = DIRECTION ( 'NONE',  ( 0.000000000000000000, 0.000000000000000000, 1.000000000000000000 ) ) ;
#13725 = CARTESIAN_POINT ( 'NONE',  ( 134.6261364156840159, -73.66016459667361005, 7.423013666676803624 ) ) ;
#13726 = DIRECTION ( 'NONE',  ( 1.000000000000000000, 0.000000000000000000, 0.000000000000000000 ) ) ;
#13727 = CARTESIAN_POINT ( 'NONE',  ( 50.93469132750264095, 59.42266395395811429, 132.4711112102474146 ) ) ;
#13728 = CARTESIAN_POINT ( 'NONE',  ( 9.564549117045082482, 62.18629025319818737, 248.9926560891072143 ) ) ;
#13729 = PLANE ( 'NONE',  #1919 ) ;
#13730 = VERTEX_POINT ( 'NONE', #6323 ) ;
#13731 = LINE ( 'NONE', #17121, #12077 ) ;
#13732 = CARTESIAN_POINT ( 'NONE',  ( -132.3557670345054191, -70.70247614046988360, 4.526726988747244107 ) ) ;
#13733 = ADVANCED_FACE ( 'NONE', ( #20220 ), #3051, .F. ) ;
#13734 = CARTESIAN_POINT ( 'NONE',  ( 130.0531662534324937, -74.83651286709024930, 0.7279510403262877682 ) ) ;
#13735 = LINE ( 'NONE', #1469, #16059 ) ;
#13736 = DIRECTION ( 'NONE',  ( -0.000000000000000000, 0.8660254037844387076, 0.4999999999999998335 ) ) ;
#13737 = CARTESIAN_POINT ( 'NONE',  ( -132.7722305162506302, -69.92010858955688946, 34.10135643643651093 ) ) ;
#13738 = ORIENTED_EDGE ( 'NONE', *, *, #11892, .F. ) ;
#13739 = ADVANCED_FACE ( 'NONE', ( #8146 ), #18594, .F. ) ;
#13740 = FACE_OUTER_BOUND ( 'NONE', #17585, .T. ) ;
#13741 = VECTOR ( 'NONE', #516, 1000.000000000000000 ) ;
#13742 = ORIENTED_EDGE ( 'NONE', *, *, #12666, .F. ) ;
#13743 = ORIENTED_EDGE ( 'NONE', *, *, #4016, .F. ) ;
#13744 = ADVANCED_FACE ( 'NONE', ( #3147 ), #17473, .F. ) ;
#13745 = ORIENTED_EDGE ( 'NONE', *, *, #3460, .T. ) ;
#13746 = DIRECTION ( 'NONE',  ( 0.000000000000000000, -1.000000000000000000, 0.000000000000000000 ) ) ;
#13747 = AXIS2_PLACEMENT_3D ( 'NONE', #12883, #5027, #12980 ) ;
#13748 = DIRECTION ( 'NONE',  ( 0.000000000000000000, -0.8660254037844379305, 0.5000000000000013323 ) ) ;
#13749 = CARTESIAN_POINT ( 'NONE',  ( 62.95000000000000284, 0.000000000000000000, 0.000000000000000000 ) ) ;
#13750 = ORIENTED_EDGE ( 'NONE', *, *, #5310, .F. ) ;
#13751 = AXIS2_PLACEMENT_3D ( 'NONE', #11989, #6189, #4750 ) ;
#13752 = CARTESIAN_POINT ( 'NONE',  ( -138.1826048463154279, -18.76197922584882960, -15.75885094356106464 ) ) ;
#13753 = CARTESIAN_POINT ( 'NONE',  ( -22.30005961346265408, -56.50329132715937419, 293.5832628385307999 ) ) ;
#13754 = ORIENTED_EDGE ( 'NONE', *, *, #19486, .T. ) ;
#13755 = CARTESIAN_POINT ( 'NONE',  ( -93.08628513671655469, 98.60439646660965707, -25.65138098760644425 ) ) ;
#13756 = CARTESIAN_POINT ( 'NONE',  ( -41.02212542604614498, -44.79787735033404061, 283.5832628385307999 ) ) ;
#13757 = CARTESIAN_POINT ( 'NONE',  ( -133.3649390995068984, -81.63041515106807822, 1.796504641981583550 ) ) ;
#13758 = APPLICATION_CONTEXT ( 'automotive_design' ) ;
#13759 = EDGE_CURVE ( 'NONE', #1551, #18312, #17264, .T. ) ;
#13760 = DIRECTION ( 'NONE',  ( 1.000000000000000000, 0.000000000000000000, 0.000000000000000000 ) ) ;
#13761 = EDGE_CURVE ( 'NONE', #12874, #8815, #9583, .T. ) ;
#13762 = EDGE_CURVE ( 'NONE', #15302, #18854, #15929, .T. ) ;
#13763 = UNCERTAINTY_MEASURE_WITH_UNIT (LENGTH_MEASURE( 1.000000000000000082E-05 ), #3711, 'distance_accuracy_value', 'NONE');
#13764 = CARTESIAN_POINT ( 'NONE',  ( 131.5441688916729390, -89.82688951536542277, 39.94263630573486523 ) ) ;
#13765 = CARTESIAN_POINT ( 'NONE',  ( 59.51523122377253117, -12.14914984460739156, 283.5832628385307999 ) ) ;
#13766 = EDGE_LOOP ( 'NONE', ( #10177, #14318, #2789, #8111 ) ) ;
#13767 = ORIENTED_EDGE ( 'NONE', *, *, #16130, .F. ) ;
#13768 = DIRECTION ( 'NONE',  ( 0.000000000000000000, 0.000000000000000000, 1.000000000000000000 ) ) ;
#13769 = ORIENTED_EDGE ( 'NONE', *, *, #15044, .F. ) ;
#13770 = ORIENTED_EDGE ( 'NONE', *, *, #17268, .F. ) ;
#13771 = CARTESIAN_POINT ( 'NONE',  ( 0.000000000000000000, 0.000000000000000000, 0.000000000000000000 ) ) ;
#13772 = EDGE_CURVE ( 'NONE', #15722, #3219, #4683, .T. ) ;
#13773 = CIRCLE ( 'NONE', #14772, 7.500000000000000000 ) ;
#13774 = EDGE_LOOP ( 'NONE', ( #12121, #179, #8398 ) ) ;
#13775 = VERTEX_POINT ( 'NONE', #15829 ) ;
#13776 = DIRECTION ( 'NONE',  ( 0.000000000000000000, 0.000000000000000000, 1.000000000000000000 ) ) ;
#13777 = DIRECTION ( 'NONE',  ( -0.9749279121818226201, -0.2225209339563185285, 0.000000000000000000 ) ) ;
#13778 = DIRECTION ( 'NONE',  ( 0.000000000000000000, 0.000000000000000000, 1.000000000000000000 ) ) ;
#13779 = EDGE_LOOP ( 'NONE', ( #5652, #3373, #17103 ) ) ;
#13780 = CARTESIAN_POINT ( 'NONE',  ( 106.6880305650188347, 105.4403344747995988, 60.00000000000000000 ) ) ;
#13781 = DIRECTION ( 'NONE',  ( 1.000000000000000000, 0.000000000000000000, 0.000000000000000000 ) ) ;
#13782 = ORIENTED_EDGE ( 'NONE', *, *, #17006, .T. ) ;
#13783 = DIRECTION ( 'NONE',  ( 0.000000000000000000, 0.000000000000000000, -1.000000000000000000 ) ) ;
#13784 = CARTESIAN_POINT ( 'NONE',  ( 49.24833719034187851, 60.83768308848395634, 248.9926560891072143 ) ) ;
#13785 = EDGE_CURVE ( 'NONE', #11258, #2863, #1810, .T. ) ;
#13786 = DIRECTION ( 'NONE',  ( -0.4338837391175651703, 0.9009688679024158153, -0.000000000000000000 ) ) ;
#13787 = VECTOR ( 'NONE', #2234, 1000.000000000000000 ) ;
#13788 = CIRCLE ( 'NONE', #11193, 10.00000000000000711 ) ;
#13789 = FACE_OUTER_BOUND ( 'NONE', #8645, .T. ) ;
#13790 = DIRECTION ( 'NONE',  ( 0.000000000000000000, 0.000000000000000000, 1.000000000000000000 ) ) ;
#13791 = CARTESIAN_POINT ( 'NONE',  ( 2.605298826209745400, 5.111158570920780519, 293.5832628385307999 ) ) ;
#13792 = EDGE_CURVE ( 'NONE', #2887, #19150, #14081, .T. ) ;
#13793 = ORIENTED_EDGE ( 'NONE', *, *, #13214, .T. ) ;
#13794 = DIRECTION ( 'NONE',  ( 0.000000000000000000, 0.000000000000000000, 1.000000000000000000 ) ) ;
#13795 = LINE ( 'NONE', #18310, #8597 ) ;
#13796 = EDGE_LOOP ( 'NONE', ( #5347, #8525, #7630, #7517 ) ) ;
#13797 = AXIS2_PLACEMENT_3D ( 'NONE', #11678, #5449, #3909 ) ;
#13798 = ORIENTED_EDGE ( 'NONE', *, *, #5757, .F. ) ;
#13799 = CARTESIAN_POINT ( 'NONE',  ( -82.35314629726805435, -125.3713054028917071, 33.70901503745690064 ) ) ;
#13800 = ORIENTED_EDGE ( 'NONE', *, *, #17919, .T. ) ;
#13801 = CARTESIAN_POINT ( 'NONE',  ( 23.22641211976290876, 56.12662799072082720, 293.5832628385307999 ) ) ;
#13802 = CARTESIAN_POINT ( 'NONE',  ( 27.53920554013639688, 73.25972925305639194, 248.9926560891072143 ) ) ;
#13803 = CIRCLE ( 'NONE', #3043, 7.500000000000007105 ) ;
#13804 = ORIENTED_EDGE ( 'NONE', *, *, #2388, .F. ) ;
#13805 = AXIS2_PLACEMENT_3D ( 'NONE', #14121, #19049, #3486 ) ;
#13806 = CARTESIAN_POINT ( 'NONE',  ( 82.42180963433075647, -125.3261898519401001, 5.922222528876336156 ) ) ;
#13807 = LINE ( 'NONE', #2773, #6379 ) ;
#13808 = VECTOR ( 'NONE', #13455, 1000.000000000000114 ) ;
#13809 = CARTESIAN_POINT ( 'NONE',  ( -141.4430087160396283, -18.68139018776262006, -13.92791448115454678 ) ) ;
#13810 = LINE ( 'NONE', #10942, #12880 ) ;
#13811 = CARTESIAN_POINT ( 'NONE',  ( 40.27908801169993325, 45.46712722958823605, 283.5832628385307999 ) ) ;
#13812 = CARTESIAN_POINT ( 'NONE',  ( -15.91767397667355510, 149.1530343478547422, 60.00000000000000000 ) ) ;
#13813 = DIRECTION ( 'NONE',  ( 0.000000000000000000, 0.000000000000000000, -1.000000000000000000 ) ) ;
#13814 = CARTESIAN_POINT ( 'NONE',  ( 89.41572940475639086, -120.4415366094430482, 45.96144366595092379 ) ) ;
#13815 = ORIENTED_EDGE ( 'NONE', *, *, #11636, .T. ) ;
#13816 = LINE ( 'NONE', #3089, #4168 ) ;
#13817 = DIRECTION ( 'NONE',  ( -0.6234898018587431423, 0.7818314824680221431, 0.000000000000000000 ) ) ;
#13818 = AXIS2_PLACEMENT_3D ( 'NONE', #9803, #4915, #8265 ) ;
#13819 = ORIENTED_EDGE ( 'NONE', *, *, #14946, .F. ) ;
#13820 = ORIENTED_EDGE ( 'NONE', *, *, #14924, .T. ) ;
#13821 = VECTOR ( 'NONE', #5661, 1000.000000000000000 ) ;
#13822 = ORIENTED_EDGE ( 'NONE', *, *, #11209, .T. ) ;
#13823 = FACE_BOUND ( 'NONE', #11110, .T. ) ;
#13824 = CIRCLE ( 'NONE', #14160, 62.91752772691707207 ) ;
#13825 = ORIENTED_EDGE ( 'NONE', *, *, #10124, .F. ) ;
#13826 = LINE ( 'NONE', #18657, #3378 ) ;
#13827 = DIRECTION ( 'NONE',  ( 0.4338837391175654479, -0.9009688679024155933, 0.000000000000000000 ) ) ;
#13828 = CARTESIAN_POINT ( 'NONE',  ( -54.89456854707563593, -30.74413178637172805, 132.4711112102474146 ) ) ;
#13829 = DIRECTION ( 'NONE',  ( -0.000000000000000000, -0.000000000000000000, -1.000000000000000000 ) ) ;
#13830 = CIRCLE ( 'NONE', #8611, 7.500000000000020428 ) ;
#13831 = FACE_OUTER_BOUND ( 'NONE', #19068, .T. ) ;
#13832 = DIRECTION ( 'NONE',  ( 0.4693298356057564180, -0.8830229359480272766, 0.000000000000000000 ) ) ;
#13833 = ORIENTED_EDGE ( 'NONE', *, *, #1304, .T. ) ;
#13834 = CARTESIAN_POINT ( 'NONE',  ( 0.000000000000000000, 0.000000000000000000, 132.4711112102474146 ) ) ;
#13835 = CARTESIAN_POINT ( 'NONE',  ( 0.000000000000000000, 0.000000000000000000, 60.00000000000000000 ) ) ;
#13836 = CARTESIAN_POINT ( 'NONE',  ( 129.7375433114042096, -75.28992114163500560, -6.767788122726502209 ) ) ;
#13837 = ADVANCED_BREP_SHAPE_REPRESENTATION ( '', ( #1054, #18639 ), #15396 ) ;
#13838 = CIRCLE ( 'NONE', #1437, 39.99999999999997868 ) ;
#13839 = DIRECTION ( 'NONE',  ( 0.9848077530122103518, -0.1736481776669172583, 0.000000000000000000 ) ) ;
#13840 = DIRECTION ( 'NONE',  ( 0.2080686897406943681, 0.9781142164131909622, 0.000000000000000000 ) ) ;
#13841 = CARTESIAN_POINT ( 'NONE',  ( -132.3553460543473932, -70.70324312376081366, 35.47401752195474245 ) ) ;
#13842 = EDGE_CURVE ( 'NONE', #14032, #3122, #170, .T. ) ;
#13843 = VERTEX_POINT ( 'NONE', #1611 ) ;
#13844 = PLANE ( 'NONE',  #16103 ) ;
#13845 = AXIS2_PLACEMENT_3D ( 'NONE', #702, #3872, #9913 ) ;
#13846 = ORIENTED_EDGE ( 'NONE', *, *, #1677, .F. ) ;
#13847 = ORIENTED_EDGE ( 'NONE', *, *, #11725, .F. ) ;
#13848 = EDGE_CURVE ( 'NONE', #13023, #18959, #6116, .T. ) ;
#13849 = VERTEX_POINT ( 'NONE', #7737 ) ;
#13850 = ADVANCED_FACE ( 'NONE', ( #12644 ), #12746, .F. ) ;
#13851 = EDGE_CURVE ( 'NONE', #6772, #11398, #9278, .T. ) ;
#13852 = LINE ( 'NONE', #17040, #17791 ) ;
#13853 = VECTOR ( 'NONE', #2513, 1000.000000000000000 ) ;
#13854 = CARTESIAN_POINT ( 'NONE',  ( -97.49999999999997158, -195.8578643762690206, 35.85786437626905609 ) ) ;
#13855 = VERTEX_POINT ( 'NONE', #17164 ) ;
#13856 = CARTESIAN_POINT ( 'NONE',  ( -76.83212392882501263, -14.94814811854935854, 132.4711112102474146 ) ) ;
#13857 = CYLINDRICAL_SURFACE ( 'NONE', #9463, 77.50000000000000000 ) ;
#13858 = ORIENTED_EDGE ( 'NONE', *, *, #15106, .T. ) ;
#13859 = FACE_OUTER_BOUND ( 'NONE', #12066, .T. ) ;
#13860 = DIRECTION ( 'NONE',  ( 1.000000000000000000, 0.000000000000000000, -0.000000000000000000 ) ) ;
#13861 = CARTESIAN_POINT ( 'NONE',  ( 176.1792632384392334, -186.5724904703758682, 10.00000000000000178 ) ) ;
#13862 = CARTESIAN_POINT ( 'NONE',  ( 0.3593302862868675285, 3.504574740656562160, 9.000000000000003553 ) ) ;
#13863 = CARTESIAN_POINT ( 'NONE',  ( 41.06890862491472660, 47.66508197439486594, 293.5832628385307999 ) ) ;
#13864 = EDGE_CURVE ( 'NONE', #13158, #5706, #15138, .T. ) ;
#13865 = CARTESIAN_POINT ( 'NONE',  ( 123.6158562626681032, -84.97727779989052976, 49.99999999947959139 ) ) ;
#13866 = AXIS2_PLACEMENT_3D ( 'NONE', #17386, #16049, #9598 ) ;
#13867 = CARTESIAN_POINT ( 'NONE',  ( -9.176097008933940202, -25.21111933077039069, 39.88498244535551862 ) ) ;
#13868 = EDGE_LOOP ( 'NONE', ( #13388, #7581, #10514 ) ) ;
#13869 = EDGE_LOOP ( 'NONE', ( #14463, #18933 ) ) ;
#13870 = DIRECTION ( 'NONE',  ( 0.3420201433256757073, -0.9396926207859057634, 0.000000000000000000 ) ) ;
#13871 = ORIENTED_EDGE ( 'NONE', *, *, #1123, .T. ) ;
#13872 = EDGE_LOOP ( 'NONE', ( #50, #7915, #2467, #12419 ) ) ;
#13873 = DIRECTION ( 'NONE',  ( 1.000000000000000000, 0.000000000000000000, 0.000000000000000000 ) ) ;
#13874 = ORIENTED_EDGE ( 'NONE', *, *, #15416, .T. ) ;
#13875 = VERTEX_POINT ( 'NONE', #3648 ) ;
#13876 = EDGE_CURVE ( 'NONE', #8342, #4330, #19399, .T. ) ;
#13877 = VECTOR ( 'NONE', #11926, 1000.000000000000114 ) ;
#13878 = EDGE_CURVE ( 'NONE', #7889, #17522, #8240, .T. ) ;
#13879 = DIRECTION ( 'NONE',  ( -0.3088643371590125697, 0.9511061040868803440, 0.000000000000000000 ) ) ;
#13880 = DIRECTION ( 'NONE',  ( 1.000000000000000000, 0.000000000000000000, 0.000000000000000000 ) ) ;
#13881 = DIRECTION ( 'NONE',  ( -0.000000000000000000, -0.000000000000000000, 1.000000000000000000 ) ) ;
#13882 = ORIENTED_EDGE ( 'NONE', *, *, #5140, .F. ) ;
#13883 = AXIS2_PLACEMENT_3D ( 'NONE', #19174, #9847, #12715 ) ;
#13884 = DIRECTION ( 'NONE',  ( 0.000000000000000000, -1.000000000000000000, -3.469446951953611231E-16 ) ) ;
#13885 = CARTESIAN_POINT ( 'NONE',  ( 97.50000000000002842, -189.9999999999999716, 30.00000000000000000 ) ) ;
#13886 = EDGE_LOOP ( 'NONE', ( #14878, #18827, #13742, #7563 ) ) ;
#13887 = PLANE ( 'NONE',  #12616 ) ;
#13888 = CARTESIAN_POINT ( 'NONE',  ( -40.27908801169994746, -45.46712722958822184, 283.5832628385307999 ) ) ;
#13889 = LINE ( 'NONE', #9080, #7338 ) ;
#13890 = ADVANCED_FACE ( 'NONE', ( #8546 ), #9878, .F. ) ;
#13891 = CARTESIAN_POINT ( 'NONE',  ( 77.50000000000000000, 0.000000000000000000, -105.0000000000000142 ) ) ;
#13892 = CARTESIAN_POINT ( 'NONE',  ( -134.3956174703911017, -75.35551001548425631, 34.63745171344068297 ) ) ;
#13893 = DIRECTION ( 'NONE',  ( -0.1736481776669273336, 0.9848077530122086864, 1.229460064647279041E-15 ) ) ;
#13894 = VERTEX_POINT ( 'NONE', #5091 ) ;
#13895 = CARTESIAN_POINT ( 'NONE',  ( -110.0000000000000142, 275.0000000000000000, 5.000000000000000888 ) ) ;
#13896 = CARTESIAN_POINT ( 'NONE',  ( 19.23677882349201695, -57.61823435390814296, 293.5832628385307999 ) ) ;
#13897 = ORIENTED_EDGE ( 'NONE', *, *, #16658, .F. ) ;
#13898 = VERTEX_POINT ( 'NONE', #12846 ) ;
#13899 = PLANE ( 'NONE',  #3225 ) ;
#13900 = EDGE_CURVE ( 'NONE', #12588, #16701, #5290, .T. ) ;
#13901 = ORIENTED_EDGE ( 'NONE', *, *, #14997, .F. ) ;
#13903 = EDGE_CURVE ( 'NONE', #7664, #4838, #9984, .T. ) ;
#13902 = AXIS2_PLACEMENT_3D ( 'NONE', #1182, #7428, #7234 ) ;
#13904 = DIRECTION ( 'NONE',  ( 0.000000000000000000, 0.000000000000000000, -1.000000000000000000 ) ) ;
#13905 = CARTESIAN_POINT ( 'NONE',  ( 0.000000000000000000, 0.000000000000000000, 283.5832628385307999 ) ) ;
#13906 = VERTEX_POINT ( 'NONE', #13133 ) ;
#13907 = AXIS2_PLACEMENT_3D ( 'NONE', #17174, #19921, #13985 ) ;
#13908 = CARTESIAN_POINT ( 'NONE',  ( 0.000000000000000000, 0.000000000000000000, 132.4711112102474146 ) ) ;
#13909 = DIRECTION ( 'NONE',  ( -0.9848077530122080203, -0.1736481776669306920, 0.000000000000000000 ) ) ;
#13910 = EDGE_CURVE ( 'NONE', #18605, #15066, #17769, .T. ) ;
#13911 = CARTESIAN_POINT ( 'NONE',  ( -110.0000000000000142, 285.0000000000000568, 5.000000000000000888 ) ) ;
#13912 = DIRECTION ( 'NONE',  ( -0.000000000000000000, -0.000000000000000000, -1.000000000000000000 ) ) ;
#13913 = VERTEX_POINT ( 'NONE', #2317 ) ;
#13914 = CARTESIAN_POINT ( 'NONE',  ( 0.000000000000000000, 0.000000000000000000, 60.00000000000000000 ) ) ;
#13915 = CARTESIAN_POINT ( 'NONE',  ( -189.9999999999988916, 285.0000000000000568, -2.499999999999734879 ) ) ;
#13916 = PLANE ( 'NONE',  #2373 ) ;
#13917 = CARTESIAN_POINT ( 'NONE',  ( 97.49999999944091655, -115.4778303847715790, 29.84273253271013360 ) ) ;
#13918 = AXIS2_PLACEMENT_3D ( 'NONE', #11301, #17558, #6706 ) ;
#13919 = ORIENTED_EDGE ( 'NONE', *, *, #7764, .T. ) ;
#13920 = VECTOR ( 'NONE', #14492, 1000.000000000000000 ) ;
#13921 = DIRECTION ( 'NONE',  ( -1.000000000000000000, -0.000000000000000000, -0.000000000000000000 ) ) ;
#13922 = DIRECTION ( 'NONE',  ( -0.000000000000000000, 0.000000000000000000, -1.000000000000000000 ) ) ;
#13923 = ORIENTED_EDGE ( 'NONE', *, *, #10212, .T. ) ;
#13925 = ORIENTED_EDGE ( 'NONE', *, *, #18489, .F. ) ;
#13924 = AXIS2_PLACEMENT_3D ( 'NONE', #16549, #2632, #8856 ) ;
#13926 = DIRECTION ( 'NONE',  ( 1.000000000000000000, 0.000000000000000000, 0.000000000000000000 ) ) ;
#13927 = ORIENTED_EDGE ( 'NONE', *, *, #5532, .F. ) ;
#13928 = CARTESIAN_POINT ( 'NONE',  ( -102.1629267457074093, -127.3823967956317347, 1.521494987488698269 ) ) ;
#13929 = CYLINDRICAL_SURFACE ( 'NONE', #1517, 7.500000000000006217 ) ;
#13930 = VERTEX_POINT ( 'NONE', #17575 ) ;
#13931 = PLANE ( 'NONE',  #8908 ) ;
#13932 = DIRECTION ( 'NONE',  ( -0.000000000000000000, -0.000000000000000000, 1.000000000000000000 ) ) ;
#13933 = CARTESIAN_POINT ( 'NONE',  ( -82.03124999999998579, -125.5821405433014348, 9.999999999999991118 ) ) ;
#13934 = VECTOR ( 'NONE', #10189, 1000.000000000000000 ) ;
#13935 = VECTOR ( 'NONE', #11571, 1000.000000000000227 ) ;
#13936 = CARTESIAN_POINT ( 'NONE',  ( -85.50395135567417526, -123.2448845699152002, 41.61540074481813178 ) ) ;
#13937 = CARTESIAN_POINT ( 'NONE',  ( -130.9868171408399462, -91.88282611735537841, 40.00000000000000000 ) ) ;
#13938 = CARTESIAN_POINT ( 'NONE',  ( 53.87178215532755132, 28.06680738835045119, 293.5832628385307999 ) ) ;
#13939 = DIRECTION ( 'NONE',  ( 0.2225209339563031519, 0.9749279121818261729, -0.000000000000000000 ) ) ;
#13940 = CARTESIAN_POINT ( 'NONE',  ( 0.000000000000000000, 0.000000000000000000, 283.5832628385307999 ) ) ;
#13941 = CARTESIAN_POINT ( 'NONE',  ( 125.9179923520548954, -81.51769904231269948, -9.421453882809895930 ) ) ;
#13942 = DIRECTION ( 'NONE',  ( -0.6692498792541777819, -0.7430374143461878633, 0.000000000000000000 ) ) ;
#13943 = PLANE ( 'NONE',  #11981 ) ;
#13944 = CARTESIAN_POINT ( 'NONE',  ( -132.0132531075724671, -71.33615934021206328, 36.30293437782199106 ) ) ;
#13945 = ORIENTED_EDGE ( 'NONE', *, *, #17492, .F. ) ;
#13946 = DIRECTION ( 'NONE',  ( -0.000000000000000000, -0.000000000000000000, 1.000000000000000000 ) ) ;
#13947 = ORIENTED_EDGE ( 'NONE', *, *, #16884, .F. ) ;
#13948 = EDGE_LOOP ( 'NONE', ( #13360, #4868, #1077, #12152 ) ) ;
#13949 = SHAPE_REPRESENTATION ( 'MOTOR', ( #18639 ), #8174 ) ;
#13950 = AXIS2_PLACEMENT_3D ( 'NONE', #1204, #12352, #4591 ) ;
#13951 = ORIENTED_EDGE ( 'NONE', *, *, #19533, .T. ) ;
#13952 = CARTESIAN_POINT ( 'NONE',  ( -143.6837422564963163, -15.75497795184483962, -4.519904249420592102 ) ) ;
#13953 = ADVANCED_FACE ( 'NONE', ( #3838 ), #14782, .F. ) ;
#13954 = CARTESIAN_POINT ( 'NONE',  ( 7.350000000000000533, 9.000000000000000000, 0.000000000000000000 ) ) ;
#13955 = DIRECTION ( 'NONE',  ( 0.000000000000000000, 0.000000000000000000, -1.000000000000000000 ) ) ;
#13956 = ORIENTED_EDGE ( 'NONE', *, *, #8135, .T. ) ;
#13957 = DIRECTION ( 'NONE',  ( -1.000000000000000000, -0.000000000000000000, -0.000000000000000000 ) ) ;
#13958 = CARTESIAN_POINT ( 'NONE',  ( 92.34802049131684498, -66.64338626758360817, 14.88498244535480630 ) ) ;
#13959 = ORIENTED_EDGE ( 'NONE', *, *, #19282, .F. ) ;
#13960 = CARTESIAN_POINT ( 'NONE',  ( -104.5717993161247676, 81.74765234771037115, -29.58341083972238295 ) ) ;
#13961 = CARTESIAN_POINT ( 'NONE',  ( 39.37628763770421614, 49.07263256785966377, 248.9926560891072143 ) ) ;
#13962 = CARTESIAN_POINT ( 'NONE',  ( -49.67518383744793908, 60.47951622432802310, 132.4711112102474146 ) ) ;
#13963 = DIRECTION ( 'NONE',  ( 0.000000000000000000, 0.000000000000000000, 1.000000000000000000 ) ) ;
#13964 = DIRECTION ( 'NONE',  ( 0.000000000000000000, 0.000000000000000000, -1.000000000000000000 ) ) ;
#13965 = VECTOR ( 'NONE', #12855, 1000.000000000000114 ) ;
#13966 = VECTOR ( 'NONE', #12324, 1000.000000000000000 ) ;
#13967 = EDGE_CURVE ( 'NONE', #7556, #18388, #12849, .T. ) ;
#13968 = CARTESIAN_POINT ( 'NONE',  ( 130.0420013710427156, -74.85033908745178621, 39.25082761537147036 ) ) ;
#13969 = CARTESIAN_POINT ( 'NONE',  ( 85.53020504959901871, -140.9188050298377846, 49.99999999999999289 ) ) ;
#13970 = ORIENTED_EDGE ( 'NONE', *, *, #7661, .T. ) ;
#13971 = EDGE_CURVE ( 'NONE', #10778, #1323, #8344, .T. ) ;
#13972 = ORIENTED_EDGE ( 'NONE', *, *, #5362, .T. ) ;
#13973 = VERTEX_POINT ( 'NONE', #20093 ) ;
#13974 = VERTEX_POINT ( 'NONE', #15183 ) ;
#13975 = DIRECTION ( 'NONE',  ( -0.5000000000000039968, 0.8660254037844363761, 0.000000000000000000 ) ) ;
#13976 = VERTEX_POINT ( 'NONE', #19788 ) ;
#13977 = CARTESIAN_POINT ( 'NONE',  ( -55.43188410062182925, -19.30071112029661151, 132.4711112102474146 ) ) ;
#13978 = CONICAL_SURFACE ( 'NONE', #6484, 79.75827554147308263, 0.5305858521701756203 ) ;
#13979 = EDGE_CURVE ( 'NONE', #961, #10982, #15810, .T. ) ;
#13980 = DIRECTION ( 'NONE',  ( -0.000000000000000000, -0.000000000000000000, 1.000000000000000000 ) ) ;
#13981 = VECTOR ( 'NONE', #718, 1000.000000000000227 ) ;
#13982 = SURFACE_STYLE_USAGE ( .BOTH. , #11923 ) ;
#13983 = CARTESIAN_POINT ( 'NONE',  ( 0.000000000000000000, 0.000000000000000000, -105.0000000000000142 ) ) ;
#13984 = EDGE_LOOP ( 'NONE', ( #3983, #9536 ) ) ;
#13985 = DIRECTION ( 'NONE',  ( 1.000000000000000000, 0.000000000000000000, 0.000000000000000000 ) ) ;
#13986 = CARTESIAN_POINT ( 'NONE',  ( 62.90240729679780429, 1.379293853802413983, 132.4711112102474146 ) ) ;
#13987 = EDGE_LOOP ( 'NONE', ( #4248, #3974, #11633 ) ) ;
#13988 = LINE ( 'NONE', #18400, #7402 ) ;
#13989 = DIRECTION ( 'NONE',  ( -0.000000000000000000, -0.000000000000000000, 1.000000000000000000 ) ) ;
#13990 = LINE ( 'NONE', #6238, #17158 ) ;
#13991 = EDGE_CURVE ( 'NONE', #7509, #19500, #1079, .T. ) ;
#13992 = AXIS2_PLACEMENT_3D ( 'NONE', #14714, #12877, #8374 ) ;
#13993 = DIRECTION ( 'NONE',  ( -0.000000000000000000, -0.000000000000000000, 1.000000000000000000 ) ) ;
#13994 = EDGE_CURVE ( 'NONE', #7604, #12459, #3403, .T. ) ;
#13995 = LINE ( 'NONE', #9298, #4932 ) ;
#13996 = CARTESIAN_POINT ( 'NONE',  ( -75.21424932920895401, 118.0797154971734386, 8.890256474989355340 ) ) ;
#13997 = VECTOR ( 'NONE', #6041, 1000.000000000000000 ) ;
#13998 = CIRCLE ( 'NONE', #12356, 15.91767397667354800 ) ;
#13999 = VERTEX_POINT ( 'NONE', #16533 ) ;
#14000 = EDGE_CURVE ( 'NONE', #17652, #5526, #4699, .T. ) ;
#14001 = AXIS2_PLACEMENT_3D ( 'NONE', #17355, #12627, #12831 ) ;
#14002 = DIRECTION ( 'NONE',  ( 0.3420201433256662704, 0.9396926207859092051, 0.000000000000000000 ) ) ;
#14003 = ORIENTED_EDGE ( 'NONE', *, *, #14979, .F. ) ;
#14004 = ORIENTED_EDGE ( 'NONE', *, *, #17746, .F. ) ;
#14005 = DIRECTION ( 'NONE',  ( 1.000000000000000000, 0.000000000000000000, 0.000000000000000000 ) ) ;
#14006 = ORIENTED_EDGE ( 'NONE', *, *, #4478, .F. ) ;
#14007 = CARTESIAN_POINT ( 'NONE',  ( -137.1611395155196931, 53.79589955330019535, -24.36911571694407996 ) ) ;
#14008 = EDGE_CURVE ( 'NONE', #15468, #3495, #7510, .T. ) ;
#14009 = DIRECTION ( 'NONE',  ( -3.320906611023727849E-16, 1.000000000000000000, 0.000000000000000000 ) ) ;
#14010 = ORIENTED_EDGE ( 'NONE', *, *, #14431, .T. ) ;
#14011 = CARTESIAN_POINT ( 'NONE',  ( 85.50395135567664795, -123.2448845699134807, -1.615400744817004464 ) ) ;
#14012 = DIRECTION ( 'NONE',  ( 0.6427876096865300370, 0.7660444431189858960, 0.000000000000000000 ) ) ;
#14013 = VECTOR ( 'NONE', #159, 1000.000000000000000 ) ;
#14014 = AXIS2_PLACEMENT_3D ( 'NONE', #997, #13463, #17380 ) ;
#14015 = CIRCLE ( 'NONE', #5213, 3.224098631618455890 ) ;
#14016 = CYLINDRICAL_SURFACE ( 'NONE', #5573, 7.500000000000006217 ) ;
#14017 = LINE ( 'NONE', #9315, #473 ) ;
#14018 = ORIENTED_EDGE ( 'NONE', *, *, #13330, .F. ) ;
#14019 = DIRECTION ( 'NONE',  ( -0.000000000000000000, -0.000000000000000000, 1.000000000000000000 ) ) ;
#14020 = CARTESIAN_POINT ( 'NONE',  ( -13.12769224524071277, -59.30917539369501412, 293.5832628385307999 ) ) ;
#14021 = EDGE_CURVE ( 'NONE', #4416, #13130, #11493, .T. ) ;
#14022 = CARTESIAN_POINT ( 'NONE',  ( 0.000000000000000000, 0.000000000000000000, -49.99999999999999289 ) ) ;
#14023 = CARTESIAN_POINT ( 'NONE',  ( 97.78884382572414324, -133.5751867743630328, 32.39323387732022752 ) ) ;
#14024 = ADVANCED_FACE ( 'NONE', ( #18569 ), #10783, .T. ) ;
#14025 = VERTEX_POINT ( 'NONE', #11295 ) ;
#14026 = EDGE_CURVE ( 'NONE', #9222, #15878, #8221, .T. ) ;
#14027 = CARTESIAN_POINT ( 'NONE',  ( -14.94814811854910452, 76.83212392882505526, 112.0427633081291816 ) ) ;
#14028 = FACE_OUTER_BOUND ( 'NONE', #12922, .T. ) ;
#14029 = ORIENTED_EDGE ( 'NONE', *, *, #10737, .T. ) ;
#14030 = AXIS2_PLACEMENT_3D ( 'NONE', #2275, #629, #16086 ) ;
#14031 = VECTOR ( 'NONE', #14471, 1000.000000000000000 ) ;
#14032 = VERTEX_POINT ( 'NONE', #3528 ) ;
#14033 = ORIENTED_EDGE ( 'NONE', *, *, #8974, .F. ) ;
#14034 = CARTESIAN_POINT ( 'NONE',  ( 0.000000000000000000, 0.000000000000000000, -4.288786813147260624 ) ) ;
#14035 = ORIENTED_EDGE ( 'NONE', *, *, #17056, .T. ) ;
#14036 = DIRECTION ( 'NONE',  ( -1.000000000000000000, 0.000000000000000000, 7.137148015447434001E-15 ) ) ;
#14037 = CARTESIAN_POINT ( 'NONE',  ( 15.91767397667354800, 164.0736214083062805, 39.99999999999999289 ) ) ;
#14038 = EDGE_CURVE ( 'NONE', #796, #19032, #13113, .T. ) ;
#14039 = ORIENTED_EDGE ( 'NONE', *, *, #4401, .F. ) ;
#14040 = APPLICATION_CONTEXT ( 'automotive_design' ) ;
#14041 = CARTESIAN_POINT ( 'NONE',  ( 28.94983032429829350, -53.40245231972188833, 293.5832628385307999 ) ) ;
#14042 = DIRECTION ( 'NONE',  ( -0.000000000000000000, -0.000000000000000000, 1.000000000000000000 ) ) ;
#14043 = LINE ( 'NONE', #11172, #13534 ) ;
#14044 = CARTESIAN_POINT ( 'NONE',  ( -88.24590234222469576, -121.2961002105598141, 44.87695375404122444 ) ) ;
#14045 = CARTESIAN_POINT ( 'NONE',  ( 62.18629025319813763, -9.564549117045302751, 248.9926560891072143 ) ) ;
#14046 = FACE_OUTER_BOUND ( 'NONE', #15979, .T. ) ;
#14047 = CARTESIAN_POINT ( 'NONE',  ( -99.70727046260189752, -112.0668231182906283, -9.975445138866367856 ) ) ;
#14048 = DIRECTION ( 'NONE',  ( 0.000000000000000000, 1.000000000000000000, 0.000000000000000000 ) ) ;
#14049 = DIRECTION ( 'NONE',  ( 1.000000000000000000, 0.000000000000000000, 0.000000000000000000 ) ) ;
#14050 = EDGE_CURVE ( 'NONE', #5404, #3300, #16011, .T. ) ;
#14051 = CARTESIAN_POINT ( 'NONE',  ( -27.53920554013687649, -73.25972925305620720, 132.4711112102474146 ) ) ;
#14052 = CARTESIAN_POINT ( 'NONE',  ( -32.50000000000000000, 3.980102097228898626E-15, -110.0000000000000000 ) ) ;
#14053 = CARTESIAN_POINT ( 'NONE',  ( -131.7304022393908269, -71.85445963696412264, 36.89128936748223708 ) ) ;
#14054 = ORIENTED_EDGE ( 'NONE', *, *, #9526, .F. ) ;
#14055 = CARTESIAN_POINT ( 'NONE',  ( -3.143238168843473623, 31.03941509555038181, 39.88498244535548309 ) ) ;
#14056 = EDGE_CURVE ( 'NONE', #12474, #14128, #10887, .T. ) ;
#14057 = VECTOR ( 'NONE', #17616, 1000.000000000000227 ) ;
#14058 = AXIS2_PLACEMENT_3D ( 'NONE', #4625, #7790, #24 ) ;
#14059 = ORIENTED_EDGE ( 'NONE', *, *, #9357, .F. ) ;
#14060 = AXIS2_PLACEMENT_3D ( 'NONE', #18972, #12708, #4957 ) ;
#14061 = VERTEX_POINT ( 'NONE', #17950 ) ;
#14062 = ORIENTED_EDGE ( 'NONE', *, *, #3994, .F. ) ;
#14063 = CARTESIAN_POINT ( 'NONE',  ( -143.2800199296550829, -16.29095325894156332, -5.878076611359963621 ) ) ;
#14064 = CARTESIAN_POINT ( 'NONE',  ( 0.3563104543936055912, -6.049278984716128349, -7.522341449313002748 ) ) ;
#14065 = LINE ( 'NONE', #10988, #3539 ) ;
#14066 = DIRECTION ( 'NONE',  ( -1.000000000000000000, 0.000000000000000000, 0.000000000000000000 ) ) ;
#14067 = VERTEX_POINT ( 'NONE', #11399 ) ;
#14068 = DIRECTION ( 'NONE',  ( -0.000000000000000000, -0.000000000000000000, 1.000000000000000000 ) ) ;
#14069 = CARTESIAN_POINT ( 'NONE',  ( 37.78325588002174840, -47.56406379474564972, 293.5832628385307999 ) ) ;
#14070 = FACE_OUTER_BOUND ( 'NONE', #2532, .T. ) ;
#14071 = LINE ( 'NONE', #7621, #1669 ) ;
#14072 = AXIS2_PLACEMENT_3D ( 'NONE', #9868, #12834, #11306 ) ;
#14073 = PLANE ( 'NONE',  #14306 ) ;
#14074 = EDGE_LOOP ( 'NONE', ( #12049, #9427, #9392, #16523 ) ) ;
#14075 = CARTESIAN_POINT ( 'NONE',  ( 134.7188131032758349, -72.93593548672635052, 30.37492054169907618 ) ) ;
#14076 = CARTESIAN_POINT ( 'NONE',  ( 59.51724408343574879, -12.14957802882732452, 293.5832628385307999 ) ) ;
#14077 = VERTEX_POINT ( 'NONE', #6602 ) ;
#14078 = ORIENTED_EDGE ( 'NONE', *, *, #17417, .T. ) ;
#14079 = EDGE_LOOP ( 'NONE', ( #9788, #15521, #4677, #2583 ) ) ;
#14080 = EDGE_LOOP ( 'NONE', ( #3557, #9402, #7064, #14582 ) ) ;
#14081 = LINE ( 'NONE', #1705, #6326 ) ;
#14082 = CIRCLE ( 'NONE', #16697, 7.500000000000020428 ) ;
#14083 = ORIENTED_EDGE ( 'NONE', *, *, #11158, .F. ) ;
#14084 = LINE ( 'NONE', #172, #15907 ) ;
#14085 = AXIS2_PLACEMENT_3D ( 'NONE', #7008, #955, #1050 ) ;
#14086 = FACE_OUTER_BOUND ( 'NONE', #2016, .T. ) ;
#14087 = CARTESIAN_POINT ( 'NONE',  ( -87.10655032386719654, -147.8252249328922687, 60.00000000000000000 ) ) ;
#14088 = DIRECTION ( 'NONE',  ( 0.000000000000000000, 0.000000000000000000, 1.000000000000000000 ) ) ;
#14089 = FACE_OUTER_BOUND ( 'NONE', #322, .T. ) ;
#14090 = ORIENTED_EDGE ( 'NONE', *, *, #12992, .F. ) ;
#14091 = CARTESIAN_POINT ( 'NONE',  ( 0.000000000000000000, 0.000000000000000000, 293.5832628385307999 ) ) ;
#14092 = DIRECTION ( 'NONE',  ( 0.000000000000000000, 0.000000000000000000, 1.000000000000000000 ) ) ;
#14093 = ORIENTED_EDGE ( 'NONE', *, *, #7118, .T. ) ;
#14094 = CARTESIAN_POINT ( 'NONE',  ( -83.77529404233767707, 120.7950752208005696, -25.22193715514223200 ) ) ;
#14095 = LINE ( 'NONE', #1822, #5856 ) ;
#14096 = CYLINDRICAL_SURFACE ( 'NONE', #15856, 3.224098631618460331 ) ;
#14097 = CARTESIAN_POINT ( 'NONE',  ( -28.94886449118903826, 53.40063514825088475, 283.5832628385307999 ) ) ;
#14098 = DIRECTION ( 'NONE',  ( 1.000000000000000000, 0.000000000000000000, 0.000000000000000000 ) ) ;
#14099 = DIRECTION ( 'NONE',  ( -0.000000000000000000, -0.000000000000000000, 1.000000000000000000 ) ) ;
#14100 = EDGE_LOOP ( 'NONE', ( #9412, #1325, #6601, #3234 ) ) ;
#14101 = ADVANCED_FACE ( 'NONE', ( #16316 ), #19476, .F. ) ;
#14102 = EDGE_CURVE ( 'NONE', #15888, #15836, #10065, .T. ) ;
#14103 = CARTESIAN_POINT ( 'NONE',  ( 178.1870518357299602, -192.0755223619198944, 35.85786437626904899 ) ) ;
#14104 = ORIENTED_EDGE ( 'NONE', *, *, #8393, .F. ) ;
#14105 = ORIENTED_EDGE ( 'NONE', *, *, #16504, .T. ) ;
#14106 = CARTESIAN_POINT ( 'NONE',  ( -38.35506425062487779, -44.43084819159262366, 248.9926560891072143 ) ) ;
#14107 = ORIENTED_EDGE ( 'NONE', *, *, #16443, .F. ) ;
#14108 = ADVANCED_FACE ( 'NONE', ( #6703 ), #12925, .F. ) ;
#14109 = CARTESIAN_POINT ( 'NONE',  ( -116.9645463067439124, 79.99640762678326666, -34.39232645276845801 ) ) ;
#14110 = EDGE_CURVE ( 'NONE', #4841, #16766, #17653, .T. ) ;
#14111 = DIRECTION ( 'NONE',  ( 1.000000000000000000, 0.000000000000000000, 0.000000000000000000 ) ) ;
#14112 = ORIENTED_EDGE ( 'NONE', *, *, #19423, .T. ) ;
#14113 = EDGE_CURVE ( 'NONE', #13644, #18605, #6995, .T. ) ;
#14114 = CARTESIAN_POINT ( 'NONE',  ( 95.47048624633011116, -116.1260213179369316, 8.021552276157979833 ) ) ;
#14115 = FACE_OUTER_BOUND ( 'NONE', #17176, .T. ) ;
#14116 = EDGE_CURVE ( 'NONE', #20199, #48, #8323, .T. ) ;
#14117 = AXIS2_PLACEMENT_3D ( 'NONE', #14359, #5059, #6590 ) ;
#14118 = DIRECTION ( 'NONE',  ( 0.8479630283625716469, -0.5300553768524345344, 0.000000000000000000 ) ) ;
#14119 = CARTESIAN_POINT ( 'NONE',  ( 55.43188410062170135, 19.30071112029698455, 111.4180192758973362 ) ) ;
#14120 = ORIENTED_EDGE ( 'NONE', *, *, #15819, .T. ) ;
#14121 = CARTESIAN_POINT ( 'NONE',  ( 0.000000000000000000, 0.000000000000000000, 293.5832628385307999 ) ) ;
#14122 = CYLINDRICAL_SURFACE ( 'NONE', #10039, 62.91752772691707207 ) ;
#14123 = DIRECTION ( 'NONE',  ( -0.2225209339563047894, -0.9749279121818258398, 0.000000000000000000 ) ) ;
#14124 = VERTEX_POINT ( 'NONE', #16411 ) ;
#14125 = EDGE_CURVE ( 'NONE', #12122, #1787, #6803, .T. ) ;
#14126 = CARTESIAN_POINT ( 'NONE',  ( 31.77187437101505196, 51.77076963420834232, 283.5832628385307999 ) ) ;
#14127 = CARTESIAN_POINT ( 'NONE',  ( -70.93787238057718980, 132.1659262131047967, 13.62312833148349434 ) ) ;
#14128 = VERTEX_POINT ( 'NONE', #8428 ) ;
#14129 = EDGE_LOOP ( 'NONE', ( #16259, #13750, #8018, #18437 ) ) ;
#14130 = EDGE_LOOP ( 'NONE', ( #14324, #16509, #16633 ) ) ;
#14131 =( LENGTH_UNIT ( ) NAMED_UNIT ( * ) SI_UNIT ( .MILLI., .METRE. ) );
#14132 = CIRCLE ( 'NONE', #6624, 62.91752772691707207 ) ;
#14133 = AXIS2_PLACEMENT_3D ( 'NONE', #546, #18030, #19272 ) ;
#14134 = EDGE_LOOP ( 'NONE', ( #6745, #2386, #4111 ) ) ;
#14135 = DIRECTION ( 'NONE',  ( -0.000000000000000000, -0.000000000000000000, 1.000000000000000000 ) ) ;
#14136 = CARTESIAN_POINT ( 'NONE',  ( -13.12769224524071277, -59.30917539369501412, 293.5832628385307999 ) ) ;
#14137 = EDGE_LOOP ( 'NONE', ( #4967, #18543, #1506, #3339 ) ) ;
#14138 = EDGE_CURVE ( 'NONE', #6223, #2409, #7298, .T. ) ;
#14139 = CIRCLE ( 'NONE', #10526, 62.91752772691707207 ) ;
#14140 = CARTESIAN_POINT ( 'NONE',  ( 0.000000000000000000, 0.000000000000000000, 49.99999999999999289 ) ) ;
#14141 = CARTESIAN_POINT ( 'NONE',  ( -109.5721339228237667, 31.03941509555038181, 14.88498244535621851 ) ) ;
#14142 = CARTESIAN_POINT ( 'NONE',  ( 135.1060089022256818, -65.16414933467422088, 30.73302420088275966 ) ) ;
#14143 = EDGE_CURVE ( 'NONE', #19280, #12693, #14171, .T. ) ;
#14144 = EDGE_CURVE ( 'NONE', #14128, #15721, #14493, .T. ) ;
#14145 = CARTESIAN_POINT ( 'NONE',  ( -95.52811048055527010, -116.1520858409645314, 31.53047640601787194 ) ) ;
#14146 = CYLINDRICAL_SURFACE ( 'NONE', #12278, 106.4288957539801004 ) ;
#14147 = CARTESIAN_POINT ( 'NONE',  ( -37.93579148621510200, -68.46530598706782200, 248.9926560891072143 ) ) ;
#14148 = PLANE ( 'NONE',  #15196 ) ;
#14149 = CARTESIAN_POINT ( 'NONE',  ( -149.9810182027019891, 2.464479588725518866, 3.727447874301266673 ) ) ;
#14150 = VECTOR ( 'NONE', #18227, 1000.000000000000114 ) ;
#14151 = AXIS2_PLACEMENT_3D ( 'NONE', #17770, #11518, #5196 ) ;
#14152 = PLANE ( 'NONE',  #374 ) ;
#14153 = DIRECTION ( 'NONE',  ( -0.3420201433256568335, -0.9396926207859127578, 0.000000000000000000 ) ) ;
#14154 = CARTESIAN_POINT ( 'NONE',  ( -124.3929425833997300, -83.83509237770859102, 49.88760530048027420 ) ) ;
#14155 = ORIENTED_EDGE ( 'NONE', *, *, #97, .T. ) ;
#14156 = EDGE_CURVE ( 'NONE', #2515, #14853, #18753, .T. ) ;
#14157 = DIRECTION ( 'NONE',  ( 0.000000000000000000, 0.000000000000000000, -1.000000000000000000 ) ) ;
#14158 = AXIS2_PLACEMENT_3D ( 'NONE', #3575, #2146, #17893 ) ;
#14159 = B_SPLINE_CURVE_WITH_KNOTS ( 'NONE', 3,
 ( #2551, #810, #19443, #909, #714, #18102, #11653, #12988, #8787, #17910, #4076, #10311, #3977, #19630, #5524, #8589, #3688, #8685, #7061, #6765, #19535, #11459, #13083, #11559, #18009, #17714, #3887, #10217, #10129, #8491 ),
 .UNSPECIFIED., .F., .F.,
 ( 4, 2, 2, 2, 2, 2, 2, 2, 2, 2, 2, 2, 2, 2, 4 ),
 ( 0.000000000000000000, 0.002172065812121079086, 0.003258098718181618413, 0.004344131624242158173, 0.008688263248484319815, 0.009774296154544852636, 0.01086032906060538719, 0.01303239487272645457, 0.01520446068484752195, 0.01737652649696859106, 0.02172065812121067377, 0.02389272393333173247, 0.02606478974545278771, 0.03040892136969489123, 0.03475305299393700170 ),
 .UNSPECIFIED. ) ;
#14160 = AXIS2_PLACEMENT_3D ( 'NONE', #16986, #17196, #2971 ) ;
#14161 = ORIENTED_EDGE ( 'NONE', *, *, #10251, .T. ) ;
#14162 = APPLICATION_CONTEXT ( 'automotive_design' ) ;
#14163 = VERTEX_POINT ( 'NONE', #13619 ) ;
#14164 = AXIS2_PLACEMENT_3D ( 'NONE', #3169, #8170, #15650 ) ;
#14165 = EDGE_LOOP ( 'NONE', ( #2600, #16528 ) ) ;
#14166 = EDGE_CURVE ( 'NONE', #13775, #9040, #14808, .T. ) ;
#14167 = EDGE_CURVE ( 'NONE', #2173, #4551, #16144, .T. ) ;
#14168 = EDGE_CURVE ( 'NONE', #18511, #19007, #10559, .T. ) ;
#14169 = DIRECTION ( 'NONE',  ( -0.000000000000000000, -0.000000000000000000, 1.000000000000000000 ) ) ;
#14170 = FACE_OUTER_BOUND ( 'NONE', #2411, .T. ) ;
#14171 = CIRCLE ( 'NONE', #122, 60.74260934110282051 ) ;
#14172 = LINE ( 'NONE', #12625, #19477 ) ;
#14173 = CARTESIAN_POINT ( 'NONE',  ( 0.000000000000000000, 0.000000000000000000, 293.5832628385307999 ) ) ;
#14174 = ADVANCED_FACE ( 'NONE', ( #5762 ), #7096, .T. ) ;
#14175 = ORIENTED_EDGE ( 'NONE', *, *, #6523, .F. ) ;
#14176 = CARTESIAN_POINT ( 'NONE',  ( 7.350000000000001421, 0.000000000000000000, 0.000000000000000000 ) ) ;
#14177 = DIRECTION ( 'NONE',  ( 0.03505990758545895342, 0.9993852124581886764, 0.000000000000000000 ) ) ;
#14178 = FACE_OUTER_BOUND ( 'NONE', #1688, .T. ) ;
#14179 = LINE ( 'NONE', #14580, #29 ) ;
#14180 = CARTESIAN_POINT ( 'NONE',  ( 7.350000000000001421, 7.794228634059940042, -4.500000000000010658 ) ) ;
#14181 = VERTEX_POINT ( 'NONE', #11978 ) ;
#14182 = CARTESIAN_POINT ( 'NONE',  ( 135.0821395827860272, -65.21370709269135091, 31.49693204037136596 ) ) ;
#14183 = CARTESIAN_POINT ( 'NONE',  ( 133.6066233479226071, -80.29760051435188473, 37.66252863624313818 ) ) ;
#14184 = ORIENTED_EDGE ( 'NONE', *, *, #16048, .T. ) ;
#14185 = ORIENTED_EDGE ( 'NONE', *, *, #2295, .F. ) ;
#14186 = VERTEX_POINT ( 'NONE', #9017 ) ;
#14187 = ORIENTED_EDGE ( 'NONE', *, *, #14835, .F. ) ;
#14188 = CARTESIAN_POINT ( 'NONE',  ( 30.53958573130908505, -50.13752642112839197, 132.4711112102474146 ) ) ;
#14189 = AXIS2_PLACEMENT_3D ( 'NONE', #9858, #16110, #11687 ) ;
#14190 = VERTEX_POINT ( 'NONE', #4017 ) ;
#14191 = DIRECTION ( 'NONE',  ( 0.000000000000000000, 0.000000000000000000, 1.000000000000000000 ) ) ;
#14192 = PLANE ( 'NONE',  #8598 ) ;
#14193 = DIRECTION ( 'NONE',  ( 0.000000000000000000, 0.000000000000000000, 1.000000000000000000 ) ) ;
#14194 = DIRECTION ( 'NONE',  ( 0.000000000000000000, 0.000000000000000000, 1.000000000000000000 ) ) ;
#14195 = CARTESIAN_POINT ( 'NONE',  ( 148.9554720520395108, -17.67108784863215121, 49.99999999999999289 ) ) ;
#14196 = ORIENTED_EDGE ( 'NONE', *, *, #1788, .F. ) ;
#14197 = LINE ( 'NONE', #9494, #14209 ) ;
#14198 = DIRECTION ( 'NONE',  ( -1.000000000000000000, -3.491481338843133355E-15, -0.000000000000000000 ) ) ;
#14199 = ORIENTED_EDGE ( 'NONE', *, *, #11850, .F. ) ;
#14200 = CARTESIAN_POINT ( 'NONE',  ( 61.98599999999999000, 7.347880794884121708E-16, -6.000000000000001776 ) ) ;
#14201 = DIRECTION ( 'NONE',  ( -0.000000000000000000, -0.000000000000000000, 1.000000000000000000 ) ) ;
#14202 = AXIS2_PLACEMENT_3D ( 'NONE', #517, #204, #8077 ) ;
#14203 = DIRECTION ( 'NONE',  ( 0.000000000000000000, -0.5000000000000018874, -0.8660254037844374864 ) ) ;
#14204 = DIRECTION ( 'NONE',  ( 1.000000000000000000, 0.000000000000000000, 0.000000000000000000 ) ) ;
#14205 = CARTESIAN_POINT ( 'NONE',  ( 100.2452644940503461, -111.5858889953167363, 50.00000000000000000 ) ) ;
#14206 = ORIENTED_EDGE ( 'NONE', *, *, #18645, .F. ) ;
#14207 = DIRECTION ( 'NONE',  ( -0.9902903945359630145, -0.1390141521205912334, 0.000000000000000000 ) ) ;
#14208 = ORIENTED_EDGE ( 'NONE', *, *, #262, .T. ) ;
#14209 = VECTOR ( 'NONE', #9889, 1000.000000000000000 ) ;
#14210 = ORIENTED_EDGE ( 'NONE', *, *, #10581, .F. ) ;
#14211 = FACE_OUTER_BOUND ( 'NONE', #5170, .T. ) ;
#14212 = VECTOR ( 'NONE', #19926, 1000.000000000000000 ) ;
#14213 = ORIENTED_EDGE ( 'NONE', *, *, #8482, .F. ) ;
#14214 = DIRECTION ( 'NONE',  ( 1.000000000000000000, 0.000000000000000000, 0.000000000000000000 ) ) ;
#14215 = LINE ( 'NONE', #198, #9926 ) ;
#14216 = ORIENTED_EDGE ( 'NONE', *, *, #6731, .F. ) ;
#14217 =( NAMED_UNIT ( * ) SI_UNIT ( $, .STERADIAN. ) SOLID_ANGLE_UNIT ( ) );
#14218 = CARTESIAN_POINT ( 'NONE',  ( 0.000000000000000000, 0.000000000000000000, 283.5832628385307999 ) ) ;
#14219 = EDGE_CURVE ( 'NONE', #5361, #1451, #2489, .T. ) ;
#14220 = DIRECTION ( 'NONE',  ( 0.000000000000000000, 0.000000000000000000, -1.000000000000000000 ) ) ;
#14221 = PRODUCT ( 'MAS-341', 'MAS-341', '', ( #2995 ) ) ;
#14222 = CIRCLE ( 'NONE', #19456, 7.500000000000000000 ) ;
#14223 = LINE ( 'NONE', #15558, #672 ) ;
#14224 = CARTESIAN_POINT ( 'NONE',  ( 0.000000000000000000, 0.000000000000000000, 132.4711112102474146 ) ) ;
#14225 = ORIENTED_EDGE ( 'NONE', *, *, #12605, .F. ) ;
#14226 = DIRECTION ( 'NONE',  ( 0.000000000000000000, 0.000000000000000000, 1.000000000000000000 ) ) ;
#14227 = DIRECTION ( 'NONE',  ( 1.000000000000000000, 0.000000000000000000, 0.000000000000000000 ) ) ;
#14228 = LINE ( 'NONE', #6570, #15029 ) ;
#14229 = CARTESIAN_POINT ( 'NONE',  ( 107.5000000000000142, -118.5063289449133492, 40.00000000000000000 ) ) ;
#14230 = ORIENTED_EDGE ( 'NONE', *, *, #5987, .F. ) ;
#14231 = EDGE_CURVE ( 'NONE', #5623, #18014, #11854, .T. ) ;
#14232 = LINE ( 'NONE', #12994, #9755 ) ;
#14233 = CARTESIAN_POINT ( 'NONE',  ( -70.22158424196186388, 132.5482456588196669, 9.581993153685951725 ) ) ;
#14234 = EDGE_CURVE ( 'NONE', #48, #18696, #8719, .T. ) ;
#14235 = ORIENTED_EDGE ( 'NONE', *, *, #11397, .T. ) ;
#14236 = AXIS2_PLACEMENT_3D ( 'NONE', #12709, #14048, #9448 ) ;
#14237 = ORIENTED_EDGE ( 'NONE', *, *, #10144, .T. ) ;
#14238 = EDGE_CURVE ( 'NONE', #4139, #12303, #5967, .T. ) ;
#14239 = ORIENTED_EDGE ( 'NONE', *, *, #1147, .T. ) ;
#14240 = STYLED_ITEM ( 'NONE', ( #17403 ), #8228 ) ;
#14241 = ORIENTED_EDGE ( 'NONE', *, *, #19969, .T. ) ;
#14242 = DIRECTION ( 'NONE',  ( 0.000000000000000000, 0.000000000000000000, -1.000000000000000000 ) ) ;
#14243 = CARTESIAN_POINT ( 'NONE',  ( -138.6264652121188590, 57.30678207472260510, 32.94515158125864218 ) ) ;
#14244 = ORIENTED_EDGE ( 'NONE', *, *, #786, .T. ) ;
#14245 = DIRECTION ( 'NONE',  ( 0.6427876096865300370, 0.7660444431189858960, 0.000000000000000000 ) ) ;
#14246 = CARTESIAN_POINT ( 'NONE',  ( 1.396592535537252080E-14, 0.000000000000000000, 43.88498244535546178 ) ) ;
#14247 = CARTESIAN_POINT ( 'NONE',  ( 128.2054629363889831, -77.87043913366069603, 48.14259967130468709 ) ) ;
#14248 = EDGE_CURVE ( 'NONE', #10, #16031, #13414, .T. ) ;
#14249 = CARTESIAN_POINT ( 'NONE',  ( -83.97601510866861929, -124.2902204837763378, 38.87704193713654632 ) ) ;
#14250 = CARTESIAN_POINT ( 'NONE',  ( 59.30917539369505675, -13.12769224524051559, 293.5832628385307999 ) ) ;
#14251 = AXIS2_PLACEMENT_3D ( 'NONE', #4767, #15912, #5075 ) ;
#14252 = CARTESIAN_POINT ( 'NONE',  ( -110.0000000000000142, 86.60254037844390496, 39.99999999999997868 ) ) ;
#14253 = LINE ( 'NONE', #11579, #3416 ) ;
#14254 = CARTESIAN_POINT ( 'NONE',  ( -148.7883939290497608, 19.65460682028593808, -5.098580071606036768 ) ) ;
#14255 = CARTESIAN_POINT ( 'NONE',  ( -57.92514141135453087, -18.28503710798565507, 283.5832628385307999 ) ) ;
#14256 = LINE ( 'NONE', #11178, #13350 ) ;
#14257 = CARTESIAN_POINT ( 'NONE',  ( -134.2478682171874027, -76.37034190854926408, 35.46671602548207858 ) ) ;
#14258 = ORIENTED_EDGE ( 'NONE', *, *, #7642, .F. ) ;
#14259 = EDGE_CURVE ( 'NONE', #11013, #12611, #12079, .T. ) ;
#14260 = CARTESIAN_POINT ( 'NONE',  ( -125.9580719609004973, 49.35695123619169777, -26.15414125452645067 ) ) ;
#14261 = EDGE_CURVE ( 'NONE', #12460, #8838, #225, .T. ) ;
#14262 = EDGE_CURVE ( 'NONE', #7038, #18698, #17107, .T. ) ;
#14263 = ORIENTED_EDGE ( 'NONE', *, *, #6874, .F. ) ;
#14264 = VECTOR ( 'NONE', #12140, 1000.000000000000114 ) ;
#14265 = VERTEX_POINT ( 'NONE', #18760 ) ;
#14266 = CIRCLE ( 'NONE', #16876, 15.91767397667354444 ) ;
#14267 = ORIENTED_EDGE ( 'NONE', *, *, #17699, .T. ) ;
#14268 = CARTESIAN_POINT ( 'NONE',  ( -144.6246557071403060, -14.56788443266039579, -0.2086646817306959945 ) ) ;
#14269 = CIRCLE ( 'NONE', #11319, 3.224098631618453670 ) ;
#14270 = EDGE_CURVE ( 'NONE', #17256, #6775, #4741, .T. ) ;
#14271 = LINE ( 'NONE', #1689, #17133 ) ;
#14272 = LINE ( 'NONE', #253, #14316 ) ;
#14273 = CARTESIAN_POINT ( 'NONE',  ( 0.1482032042127258142, 2.204400401860216796, -9.000000000000005329 ) ) ;
#14274 = ORIENTED_EDGE ( 'NONE', *, *, #19474, .T. ) ;
#14275 = CYLINDRICAL_SURFACE ( 'NONE', #6513, 62.91752772691707207 ) ;
#14276 = LINE ( 'NONE', #3331, #19992 ) ;
#14277 = DIRECTION ( 'NONE',  ( -0.7881095627315599650, -0.6155349844899714595, 0.000000000000000000 ) ) ;
#14278 = FACE_OUTER_BOUND ( 'NONE', #6840, .T. ) ;
#14279 = DIRECTION ( 'NONE',  ( 0.000000000000000000, 0.000000000000000000, -1.000000000000000000 ) ) ;
#14280 = VECTOR ( 'NONE', #6001, 1000.000000000000000 ) ;
#14281 = EDGE_LOOP ( 'NONE', ( #9734, #9783, #366 ) ) ;
#14282 = EDGE_CURVE ( 'NONE', #15923, #7403, #18545, .T. ) ;
#14283 = CARTESIAN_POINT ( 'NONE',  ( 132.7769743428758886, -69.91161917917226276, 34.10605816523012379 ) ) ;
#14284 = EDGE_CURVE ( 'NONE', #1745, #11508, #20050, .T. ) ;
#14285 = DIRECTION ( 'NONE',  ( -0.000000000000000000, -0.000000000000000000, 1.000000000000000000 ) ) ;
#14286 = EDGE_CURVE ( 'NONE', #3178, #18381, #15473, .T. ) ;
#14287 = ORIENTED_EDGE ( 'NONE', *, *, #16525, .T. ) ;
#14289 = ORIENTED_EDGE ( 'NONE', *, *, #3259, .F. ) ;
#14288 = VECTOR ( 'NONE', #11744, 1000.000000000000114 ) ;
#14290 = ORIENTED_EDGE ( 'NONE', *, *, #7093, .F. ) ;
#14291 = EDGE_LOOP ( 'NONE', ( #19424, #7617, #6474, #11743 ) ) ;
#14292 = EDGE_CURVE ( 'NONE', #11511, #16204, #7972, .T. ) ;
#14293 = DIRECTION ( 'NONE',  ( 0.3747554100459959958, 0.9271237148521535021, 0.000000000000000000 ) ) ;
#14294 = ADVANCED_FACE ( 'NONE', ( #12598 ), #7801, .F. ) ;
#14295 = ORIENTED_EDGE ( 'NONE', *, *, #13385, .T. ) ;
#14296 = CARTESIAN_POINT ( 'NONE',  ( 26.85905058935142975, 1.464553941565464035, 14.88498244535526460 ) ) ;
#14297 = CARTESIAN_POINT ( 'NONE',  ( -105.6231002115456903, -121.8324894761443886, 39.87517067041968488 ) ) ;
#14298 = FACE_OUTER_BOUND ( 'NONE', #14465, .T. ) ;
#14299 = CARTESIAN_POINT ( 'NONE',  ( -44.79787735033389851, 41.02212542604627998, 283.5832628385307999 ) ) ;
#14300 = EDGE_LOOP ( 'NONE', ( #19682, #1610, #17651, #3702 ) ) ;
#14301 = DIRECTION ( 'NONE',  ( 0.000000000000000000, 1.000000000000000000, 0.000000000000000000 ) ) ;
#14302 = CARTESIAN_POINT ( 'NONE',  ( -189.9999999999988916, 265.0000000000000000, 5.000000000000268230 ) ) ;
#14303 = VECTOR ( 'NONE', #4792, 1000.000000000000114 ) ;
#14304 = VERTEX_POINT ( 'NONE', #9544 ) ;
#14305 = VECTOR ( 'NONE', #10818, 1000.000000000000000 ) ;
#14306 = AXIS2_PLACEMENT_3D ( 'NONE', #18692, #2933, #9163 ) ;
#14307 = CARTESIAN_POINT ( 'NONE',  ( -98.33690426217857805, 103.1883475260306398, -33.27187555683841680 ) ) ;
#14308 = DIRECTION ( 'NONE',  ( 0.9749279121818226201, 0.2225209339563185562, 0.000000000000000000 ) ) ;
#14309 = PLANE ( 'NONE',  #3106 ) ;
#14310 = FACE_OUTER_BOUND ( 'NONE', #3160, .T. ) ;
#14311 = DIRECTION ( 'NONE',  ( -0.000000000000000000, -1.000000000000000000, -0.000000000000000000 ) ) ;
#14312 = DIRECTION ( 'NONE',  ( 0.9749279121818227312, 0.2225209339563182509, 0.000000000000000000 ) ) ;
#14313 = ORIENTED_EDGE ( 'NONE', *, *, #6, .T. ) ;
#14314 = LINE ( 'NONE', #16257, #13166 ) ;
#14315 = ORIENTED_EDGE ( 'NONE', *, *, #13330, .T. ) ;
#14316 = VECTOR ( 'NONE', #4971, 1000.000000000000000 ) ;
#14317 = EDGE_CURVE ( 'NONE', #15888, #16227, #1767, .T. ) ;
#14318 = ORIENTED_EDGE ( 'NONE', *, *, #13128, .T. ) ;
#14319 = DIRECTION ( 'NONE',  ( 0.8660254037844345998, 0.5000000000000069944, 0.000000000000000000 ) ) ;
#14320 = VECTOR ( 'NONE', #15511, 1000.000000000000000 ) ;
#14321 = ORIENTED_EDGE ( 'NONE', *, *, #5614, .F. ) ;
#14322 = DIRECTION ( 'NONE',  ( -3.129754055707530415E-16, 1.000000000000000000, -0.000000000000000000 ) ) ;
#14323 = PLANE ( 'NONE',  #5034 ) ;
#14324 = ORIENTED_EDGE ( 'NONE', *, *, #18046, .T. ) ;
#14325 = FILL_AREA_STYLE_COLOUR ( '', #2808 ) ;
#14326 = DIRECTION ( 'NONE',  ( 1.000000000000000000, 0.000000000000000000, 0.000000000000000000 ) ) ;
#14327 = LINE ( 'NONE', #9712, #11788 ) ;
#14328 = VECTOR ( 'NONE', #8769, 1000.000000000000000 ) ;
#14329 = AXIS2_PLACEMENT_3D ( 'NONE', #6903, #8326, #5562 ) ;
#14330 = DIRECTION ( 'NONE',  ( -1.000000000000000000, 0.000000000000000000, 0.000000000000000000 ) ) ;
#14331 = CARTESIAN_POINT ( 'NONE',  ( 0.000000000000000000, 0.000000000000000000, 0.000000000000000000 ) ) ;
#14332 = AXIS2_PLACEMENT_3D ( 'NONE', #5238, #9725, #17717 ) ;
#14333 = ORIENTED_EDGE ( 'NONE', *, *, #13591, .F. ) ;
#14334 = DIRECTION ( 'NONE',  ( -0.7660444431189726844, -0.6427876096865456912, 0.000000000000000000 ) ) ;
#14335 = FACE_OUTER_BOUND ( 'NONE', #15453, .T. ) ;
#14336 = LINE ( 'NONE', #9527, #6872 ) ;
#14337 = DIRECTION ( 'NONE',  ( 0.000000000000000000, 0.000000000000000000, 1.000000000000000000 ) ) ;
#14338 = ORIENTED_EDGE ( 'NONE', *, *, #19019, .T. ) ;
#14339 = DIRECTION ( 'NONE',  ( 6.982962677686266711E-15, -0.000000000000000000, 1.000000000000000000 ) ) ;
#14340 = CARTESIAN_POINT ( 'NONE',  ( 100.5989061668484226, 55.02415981988612970, 39.88498244535475123 ) ) ;
#14341 = ORIENTED_EDGE ( 'NONE', *, *, #9279, .F. ) ;
#14342 = EDGE_CURVE ( 'NONE', #3335, #5555, #4529, .T. ) ;
#14343 = ORIENTED_EDGE ( 'NONE', *, *, #348, .T. ) ;
#14344 = ORIENTED_EDGE ( 'NONE', *, *, #1094, .F. ) ;
#14345 = CONTEXT_DEPENDENT_SHAPE_REPRESENTATION ( #1212, #12747 ) ;
#14346 = VECTOR ( 'NONE', #10287, 1000.000000000000000 ) ;
#14347 = VERTEX_POINT ( 'NONE', #17015 ) ;
#14348 = AXIS2_PLACEMENT_3D ( 'NONE', #7589, #18345, #514 ) ;
#14349 = DIRECTION ( 'NONE',  ( 0.5300553768524375320, 0.8479630283625697595, 0.000000000000000000 ) ) ;
#14350 = LINE ( 'NONE', #11166, #16245 ) ;
#14351 = VERTEX_POINT ( 'NONE', #4846 ) ;
#14352 = FACE_OUTER_BOUND ( 'NONE', #10304, .T. ) ;
#14353 = CARTESIAN_POINT ( 'NONE',  ( -1.289614712049159007, 5.590028426173815568, 293.5832628385307999 ) ) ;
#14354 = CARTESIAN_POINT ( 'NONE',  ( -76.92888220842476699, 14.39940464655786201, 248.9926560891072143 ) ) ;
#14355 = EDGE_CURVE ( 'NONE', #8563, #7173, #4712, .T. ) ;
#14356 = VECTOR ( 'NONE', #3809, 1000.000000000000000 ) ;
#14357 = CARTESIAN_POINT ( 'NONE',  ( -98.09575606592595420, -113.4800522715664641, -9.802334794049597733 ) ) ;
#14358 = CYLINDRICAL_SURFACE ( 'NONE', #18767, 62.91752772691707207 ) ;
#14359 = CARTESIAN_POINT ( 'NONE',  ( 7.950000000000000178, 0.000000000000000000, 0.000000000000000000 ) ) ;
#14360 = DIRECTION ( 'NONE',  ( 1.000000000000000000, 0.000000000000000000, 0.000000000000000000 ) ) ;
#14361 = CYLINDRICAL_SURFACE ( 'NONE', #9843, 60.74260934110282051 ) ;
#14362 = VECTOR ( 'NONE', #17923, 1000.000000000000000 ) ;
#14363 = CARTESIAN_POINT ( 'NONE',  ( 0.000000000000000000, 0.000000000000000000, -39.99999999999999289 ) ) ;
#14364 = AXIS2_PLACEMENT_3D ( 'NONE', #12759, #16241, #19212 ) ;
#14365 = VERTEX_POINT ( 'NONE', #4953 ) ;
#14366 = DIRECTION ( 'NONE',  ( 0.000000000000000000, 0.000000000000000000, 1.000000000000000000 ) ) ;
#14367 = EDGE_CURVE ( 'NONE', #998, #9378, #8298, .T. ) ;
#14368 = EDGE_LOOP ( 'NONE', ( #9196, #19427, #12760, #14829, #12235, #12479 ) ) ;
#14369 = ORIENTED_EDGE ( 'NONE', *, *, #8360, .T. ) ;
#14370 = ORIENTED_EDGE ( 'NONE', *, *, #15155, .F. ) ;
#14371 = CIRCLE ( 'NONE', #319, 62.91752772691707207 ) ;
#14372 = AXIS2_PLACEMENT_3D ( 'NONE', #13545, #4346, #19794 ) ;
#14373 = CARTESIAN_POINT ( 'NONE',  ( -3.892963425580764358E-15, -7.351593252548091151, -5.266666970006173898 ) ) ;
#14374 = ADVANCED_FACE ( 'NONE', ( #31 ), #1358, .F. ) ;
#14375 = DIRECTION ( 'NONE',  ( 1.000000000000000000, 0.000000000000000000, 0.000000000000000000 ) ) ;
#14376 = CARTESIAN_POINT ( 'NONE',  ( -1.379293853801755176, 62.90240729679781850, 132.4711112102474146 ) ) ;
#14377 = EDGE_CURVE ( 'NONE', #2297, #10955, #10860, .T. ) ;
#14378 = CARTESIAN_POINT ( 'NONE',  ( 0.000000000000000000, 0.000000000000000000, 39.99999999999999289 ) ) ;
#14379 = CARTESIAN_POINT ( 'NONE',  ( -0.4239815141812765531, 0.2650276884262135479, 283.5832628385307999 ) ) ;
#14380 = DIRECTION ( 'NONE',  ( -0.000000000000000000, -0.000000000000000000, 1.000000000000000000 ) ) ;
#14381 = CARTESIAN_POINT ( 'NONE',  ( 106.5742148451190019, -120.1859338240075203, 39.99999999999999289 ) ) ;
#14382 = CARTESIAN_POINT ( 'NONE',  ( -189.9999999999988916, 275.0000000000000000, 12.50000000000027178 ) ) ;
#14383 = ORIENTED_EDGE ( 'NONE', *, *, #3002, .T. ) ;
#14384 =( GEOMETRIC_REPRESENTATION_CONTEXT ( 3 ) GLOBAL_UNCERTAINTY_ASSIGNED_CONTEXT ( ( #7851 ) ) GLOBAL_UNIT_ASSIGNED_CONTEXT ( ( #10342, #10542, #11776 ) ) REPRESENTATION_CONTEXT ( 'NONE', 'WORKASPACE' ) );
#14385 = CARTESIAN_POINT ( 'NONE',  ( 132.5095042660555293, -70.41495930837207595, 35.02927749617933273 ) ) ;
#14386 = CARTESIAN_POINT ( 'NONE',  ( 0.000000000000000000, 0.000000000000000000, -105.0000000000000142 ) ) ;
#14387 = ORIENTED_EDGE ( 'NONE', *, *, #6031, .F. ) ;
#14388 = VERTEX_POINT ( 'NONE', #3102 ) ;
#14389 = EDGE_CURVE ( 'NONE', #15683, #13913, #9334, .T. ) ;
#14390 = VERTEX_POINT ( 'NONE', #1671 ) ;
#14391 = ORIENTED_EDGE ( 'NONE', *, *, #7181, .T. ) ;
#14392 = ORIENTED_EDGE ( 'NONE', *, *, #8347, .F. ) ;
#14393 = CARTESIAN_POINT ( 'NONE',  ( -17.24542129382122724, 20.55229278271246329, 14.88498244535557369 ) ) ;
#14394 = DIRECTION ( 'NONE',  ( -0.6427876096865328126, -0.7660444431189835646, 0.000000000000000000 ) ) ;
#14395 = DIRECTION ( 'NONE',  ( -0.000000000000000000, -0.000000000000000000, 1.000000000000000000 ) ) ;
#14396 = CARTESIAN_POINT ( 'NONE',  ( -166.7850001792984926, -190.0000000000000284, 40.00000000000000000 ) ) ;
#14397 = ORIENTED_EDGE ( 'NONE', *, *, #13406, .T. ) ;
#14398 = EDGE_CURVE ( 'NONE', #5578, #2667, #13838, .T. ) ;
#14399 = VECTOR ( 'NONE', #10993, 1000.000000000000000 ) ;
#14400 = CARTESIAN_POINT ( 'NONE',  ( 129.8775639978177026, -75.04816271247871384, -6.616949551716221123 ) ) ;
#14401 = CARTESIAN_POINT ( 'NONE',  ( 1.379293853801755176, -78.26059000578311498, 132.4711112102474146 ) ) ;
#14402 = ADVANCED_FACE ( 'NONE', ( #17332 ), #9736, .F. ) ;
#14403 = ORIENTED_EDGE ( 'NONE', *, *, #14857, .T. ) ;
#14404 = LINE ( 'NONE', #6637, #7077 ) ;
#14405 = CARTESIAN_POINT ( 'NONE',  ( 0.000000000000000000, 0.000000000000000000, 283.5832628385307999 ) ) ;
#14406 = PLANE ( 'NONE',  #16372 ) ;
#14407 = DIRECTION ( 'NONE',  ( 0.000000000000000000, 0.000000000000000000, 1.000000000000000000 ) ) ;
#14408 = LINE ( 'NONE', #9599, #16579 ) ;
#14409 = FACE_OUTER_BOUND ( 'NONE', #6300, .T. ) ;
#14410 = CARTESIAN_POINT ( 'NONE',  ( 2.629250726500717672, 60.68567895461850981, 283.5832628385307999 ) ) ;
#14411 = VERTEX_POINT ( 'NONE', #8407 ) ;
#14412 = AXIS2_PLACEMENT_3D ( 'NONE', #3036, #4774, #18474 ) ;
#14413 = EDGE_CURVE ( 'NONE', #6318, #16710, #5710, .T. ) ;
#14414 = CARTESIAN_POINT ( 'NONE',  ( 0.000000000000000000, 0.000000000000000000, 283.5832628385307999 ) ) ;
#14415 = ADVANCED_FACE ( 'NONE', ( #1976, #12808, #14747, #1868, #8098, #2279 ), #5248, .F. ) ;
#14416 = ORIENTED_EDGE ( 'NONE', *, *, #6731, .T. ) ;
#14417 = CIRCLE ( 'NONE', #4951, 15.91767397667354444 ) ;
#14418 = ORIENTED_EDGE ( 'NONE', *, *, #12485, .T. ) ;
#14419 = CYLINDRICAL_SURFACE ( 'NONE', #17288, 150.0000000000000284 ) ;
#14420 = ORIENTED_EDGE ( 'NONE', *, *, #5875, .F. ) ;
#14421 = FACE_OUTER_BOUND ( 'NONE', #20016, .T. ) ;
#14422 = DIRECTION ( 'NONE',  ( 0.1390141521205946196, -0.9902903945359624593, 0.000000000000000000 ) ) ;
#14423 = ORIENTED_EDGE ( 'NONE', *, *, #12083, .T. ) ;
#14424 = EDGE_CURVE ( 'NONE', #11394, #6348, #19071, .T. ) ;
#14425 = CARTESIAN_POINT ( 'NONE',  ( -5.111158570922238020, 2.605298826210300511, 293.5832628385307999 ) ) ;
#14426 = CARTESIAN_POINT ( 'NONE',  ( 144.1130761623740568, -69.50842595698583182, 30.00000000000000000 ) ) ;
#14427 = CARTESIAN_POINT ( 'NONE',  ( -31.77296517111735596, -51.77251465595229263, 293.5832628385307999 ) ) ;
#14428 = VECTOR ( 'NONE', #19868, 1000.000000000000000 ) ;
#14429 = CARTESIAN_POINT ( 'NONE',  ( 0.000000000000000000, 0.000000000000000000, 132.4711112102474146 ) ) ;
#14430 = VECTOR ( 'NONE', #14943, 1000.000000000000114 ) ;
#14431 = EDGE_CURVE ( 'NONE', #219, #16961, #6879, .T. ) ;
#14432 = CARTESIAN_POINT ( 'NONE',  ( 18.77710619359078947, 55.62246070845787216, 132.4711112102474146 ) ) ;
#14433 = CARTESIAN_POINT ( 'NONE',  ( -58.83691981461618781, 22.28973221005139749, 132.4711112102474146 ) ) ;
#14434 = DIRECTION ( 'NONE',  ( 0.6427876096865456912, -0.7660444431189726844, 0.000000000000000000 ) ) ;
#14435 = DIRECTION ( 'NONE',  ( -0.000000000000000000, -0.000000000000000000, 1.000000000000000000 ) ) ;
#14436 = CARTESIAN_POINT ( 'NONE',  ( 60.72279549541555355, -1.629937663769388090, 293.5832628385307999 ) ) ;
#14437 = DIRECTION ( 'NONE',  ( -1.000000000000000000, 0.000000000000000000, 6.976128451377902853E-15 ) ) ;
#14438 = VERTEX_POINT ( 'NONE', #14353 ) ;
#14439 = DIRECTION ( 'NONE',  ( 1.000000000000000000, 0.000000000000000000, 0.000000000000000000 ) ) ;
#14440 = DIRECTION ( 'NONE',  ( 0.000000000000000000, 0.000000000000000000, -1.000000000000000000 ) ) ;
#14441 = ORIENTED_EDGE ( 'NONE', *, *, #2363, .F. ) ;
#14442 = EDGE_LOOP ( 'NONE', ( #119, #11107 ) ) ;
#14443 = ORIENTED_EDGE ( 'NONE', *, *, #12233, .F. ) ;
#14444 = ITEM_DEFINED_TRANSFORMATION ( 'NONE', 'NONE', #14058,  #18639 ) ;
#14445 = ORIENTED_EDGE ( 'NONE', *, *, #17235, .T. ) ;
#14446 = LINE ( 'NONE', #17530, #5224 ) ;
#14447 = CARTESIAN_POINT ( 'NONE',  ( -148.9537812787172300, 17.82720812061743842, 14.16315103253250918 ) ) ;
#14448 = EDGE_LOOP ( 'NONE', ( #20064, #20190, #11797, #7706 ) ) ;
#14449 = VECTOR ( 'NONE', #336, 1000.000000000000000 ) ;
#14450 = CARTESIAN_POINT ( 'NONE',  ( 156.4179374840099683, -52.02840013023883614, 49.99999999999999289 ) ) ;
#14451 = CARTESIAN_POINT ( 'NONE',  ( 0.1469846612282503517, 8.891930899535431365, 2.598723904613013946 ) ) ;
#14452 = CARTESIAN_POINT ( 'NONE',  ( -103.8725996235353222, -124.7053175801541158, 0.6763943681471633607 ) ) ;
#14453 = CARTESIAN_POINT ( 'NONE',  ( -133.5605114351387499, 42.14324244569257871, 30.93267679371781043 ) ) ;
#14454 = LINE ( 'NONE', #15793, #6352 ) ;
#14455 = CARTESIAN_POINT ( 'NONE',  ( -5.951998377315654842, -25.21111933077039069, 14.88498244535549198 ) ) ;
#14456 = FACE_OUTER_BOUND ( 'NONE', #12378, .T. ) ;
#14457 = DIRECTION ( 'NONE',  ( -1.000000000000000000, 0.000000000000000000, 0.000000000000000000 ) ) ;
#14458 = DIRECTION ( 'NONE',  ( 0.000000000000000000, 0.000000000000000000, -1.000000000000000000 ) ) ;
#14459 = EDGE_LOOP ( 'NONE', ( #15256, #19515 ) ) ;
#14460 = CARTESIAN_POINT ( 'NONE',  ( -134.1501013333374033, 33.24937751378277540, -20.37878451202398367 ) ) ;
#14461 = VECTOR ( 'NONE', #11181, 1000.000000000000000 ) ;
#14462 = AXIS2_PLACEMENT_3D ( 'NONE', #13914, #13603, #4098 ) ;
#14463 = ORIENTED_EDGE ( 'NONE', *, *, #2284, .T. ) ;
#14464 = ORIENTED_EDGE ( 'NONE', *, *, #1083, .T. ) ;
#14465 = EDGE_LOOP ( 'NONE', ( #11836, #1757, #16388, #10152 ) ) ;
#14466 = CARTESIAN_POINT ( 'NONE',  ( 159.9599531637113330, -36.50981547336952104, 49.99999999999999289 ) ) ;
#14467 = DIRECTION ( 'NONE',  ( 0.9396926207859046531, 0.3420201433256790380, 0.000000000000000000 ) ) ;
#14468 = AXIS2_PLACEMENT_3D ( 'NONE', #14757, #19370, #8617 ) ;
#14469 = DIRECTION ( 'NONE',  ( -0.000000000000000000, -0.000000000000000000, 1.000000000000000000 ) ) ;
#14470 = CIRCLE ( 'NONE', #19686, 17.50000000000001066 ) ;
#14471 = DIRECTION ( 'NONE',  ( 0.000000000000000000, 0.000000000000000000, 1.000000000000000000 ) ) ;
#14472 = EDGE_CURVE ( 'NONE', #2129, #18497, #11274, .T. ) ;
#14473 = DIRECTION ( 'NONE',  ( -0.000000000000000000, -0.000000000000000000, 1.000000000000000000 ) ) ;
#14474 = LINE ( 'NONE', #17661, #1706 ) ;
#14475 = DIRECTION ( 'NONE',  ( 0.1390141521205912056, -0.9902903945359629034, 0.000000000000000000 ) ) ;
#14476 = AXIS2_PLACEMENT_3D ( 'NONE', #12438, #9680, #11109 ) ;
#14477 = CARTESIAN_POINT ( 'NONE',  ( 113.3640620605771261, -25.59923667990641150, 39.88498244535465886 ) ) ;
#14478 = CYLINDRICAL_SURFACE ( 'NONE', #14942, 7.500000000000000000 ) ;
#14479 = VERTEX_POINT ( 'NONE', #728 ) ;
#14480 = EDGE_CURVE ( 'NONE', #10368, #675, #5056, .T. ) ;
#14481 = FACE_OUTER_BOUND ( 'NONE', #14134, .T. ) ;
#14482 = VERTEX_POINT ( 'NONE', #6973 ) ;
#14483 = VERTEX_POINT ( 'NONE', #3606 ) ;
#14484 = EDGE_CURVE ( 'NONE', #10450, #8591, #5047, .T. ) ;
#14485 = AXIS2_PLACEMENT_3D ( 'NONE', #92, #11233, #5015 ) ;
#14486 = EDGE_LOOP ( 'NONE', ( #5215, #4243, #8337, #13972 ) ) ;
#14487 = EDGE_CURVE ( 'NONE', #9275, #5133, #14508, .T. ) ;
#14488 = ORIENTED_EDGE ( 'NONE', *, *, #639, .F. ) ;
#14489 = EDGE_CURVE ( 'NONE', #2170, #19703, #13507, .T. ) ;
#14490 = DIRECTION ( 'NONE',  ( -0.1390141521205912334, 0.9902903945359629034, 0.000000000000000000 ) ) ;
#14491 = ORIENTED_EDGE ( 'NONE', *, *, #20172, .F. ) ;
#14492 = DIRECTION ( 'NONE',  ( -0.000000000000000000, -0.000000000000000000, 1.000000000000000000 ) ) ;
#14493 = CIRCLE ( 'NONE', #8603, 15.91767397667354444 ) ;
#14494 = DIRECTION ( 'NONE',  ( 0.000000000000000000, 0.000000000000000000, 1.000000000000000000 ) ) ;
#14495 = CARTESIAN_POINT ( 'NONE',  ( -3.453261854572980738, -4.581103194069957141, 293.5832628385307999 ) ) ;
#14496 = VECTOR ( 'NONE', #14619, 1000.000000000000000 ) ;
#14497 = CARTESIAN_POINT ( 'NONE',  ( 0.000000000000000000, 164.0736214083062805, 49.99999999999999289 ) ) ;
#14498 = ORIENTED_EDGE ( 'NONE', *, *, #4589, .F. ) ;
#14499 = CARTESIAN_POINT ( 'NONE',  ( 127.1451880273207280, -79.59002392720331898, -8.837124157530666935 ) ) ;
#14500 = LINE ( 'NONE', #6634, #19574 ) ;
#14501 = EDGE_CURVE ( 'NONE', #14685, #7508, #14557, .T. ) ;
#14502 = ORIENTED_EDGE ( 'NONE', *, *, #15234, .T. ) ;
#14503 = LINE ( 'NONE', #11222, #859 ) ;
#14504 = DIRECTION ( 'NONE',  ( -6.982962677686265922E-15, -3.944304526105059903E-31, -1.000000000000000000 ) ) ;
#14505 = CARTESIAN_POINT ( 'NONE',  ( -11.73417718768092044, -61.81362617575096152, 293.5832628385307999 ) ) ;
#14506 = CARTESIAN_POINT ( 'NONE',  ( 59.51523122377252406, -12.14914984460739156, 293.5832628385307999 ) ) ;
#14507 = CARTESIAN_POINT ( 'NONE',  ( 107.5000000000000284, -199.9999999999999716, 40.00000000000000000 ) ) ;
#14508 = CIRCLE ( 'NONE', #11568, 60.74260934110282051 ) ;
#14509 = DIRECTION ( 'NONE',  ( 6.982962677686266711E-15, -0.000000000000000000, 1.000000000000000000 ) ) ;
#14510 = CARTESIAN_POINT ( 'NONE',  ( 96.48501399889538277, -114.8592206156971116, 49.50259502882540374 ) ) ;
#14511 = VERTEX_POINT ( 'NONE', #9944 ) ;
#14512 = CARTESIAN_POINT ( 'NONE',  ( 170.2125097089226529, -199.3942630591406839, 40.00000000000000000 ) ) ;
#14513 = VECTOR ( 'NONE', #868, 1000.000000000000000 ) ;
#14514 = EDGE_LOOP ( 'NONE', ( #17673, #10851, #6963, #1832 ) ) ;
#14515 = ADVANCED_FACE ( 'NONE', ( #436 ), #19160, .F. ) ;
#14516 = ORIENTED_EDGE ( 'NONE', *, *, #16393, .T. ) ;
#14517 = EDGE_CURVE ( 'NONE', #9431, #14685, #4379, .T. ) ;
#14518 = CARTESIAN_POINT ( 'NONE',  ( 7.350000000000000533, 9.000000000000000000, 0.000000000000000000 ) ) ;
#14519 = ORIENTED_EDGE ( 'NONE', *, *, #9915, .T. ) ;
#14520 = CARTESIAN_POINT ( 'NONE',  ( 71.18887634719571622, -147.8252249328912740, 39.99999999999999289 ) ) ;
#14521 = DIRECTION ( 'NONE',  ( 0.000000000000000000, 0.000000000000000000, 1.000000000000000000 ) ) ;
#14522 = VECTOR ( 'NONE', #11742, 1000.000000000000000 ) ;
#14523 = DIRECTION ( 'NONE',  ( 6.982962677686266711E-15, -0.000000000000000000, 1.000000000000000000 ) ) ;
#14524 = CARTESIAN_POINT ( 'NONE',  ( -175.8776271403844191, -36.50981547337168109, 49.99999999999999289 ) ) ;
#14525 = LINE ( 'NONE', #17016, #369 ) ;
#14526 = EDGE_CURVE ( 'NONE', #13023, #15125, #7309, .T. ) ;
#14527 = CARTESIAN_POINT ( 'NONE',  ( 0.000000000000000000, 0.000000000000000000, 248.9926560891072143 ) ) ;
#14528 = CARTESIAN_POINT ( 'NONE',  ( -60.22029172860437285, -7.948651060879224239, 283.5832628385307999 ) ) ;
#14529 = FACE_OUTER_BOUND ( 'NONE', #4285, .T. ) ;
#14530 = DIRECTION ( 'NONE',  ( 1.000000000000000000, 0.000000000000000000, 0.000000000000000000 ) ) ;
#14531 = DIRECTION ( 'NONE',  ( 1.000000000000000000, 0.000000000000000000, -6.994638739193269649E-15 ) ) ;
#14532 = FACE_OUTER_BOUND ( 'NONE', #4831, .T. ) ;
#14533 = AXIS2_PLACEMENT_3D ( 'NONE', #1977, #10861, #7898 ) ;
#14534 = CARTESIAN_POINT ( 'NONE',  ( 45.46712722958809394, -40.27908801170008246, 283.5832628385307999 ) ) ;
#14535 = EDGE_LOOP ( 'NONE', ( #3579, #7328, #17144, #18316 ) ) ;
#14536 = CARTESIAN_POINT ( 'NONE',  ( -32.16802499836779106, -54.07248341783242296, 293.5832628385307999 ) ) ;
#14537 = DIRECTION ( 'NONE',  ( 0.000000000000000000, 0.000000000000000000, 1.000000000000000000 ) ) ;
#14538 = EDGE_CURVE ( 'NONE', #12174, #12822, #16194, .T. ) ;
#14539 = EDGE_LOOP ( 'NONE', ( #16719, #7823, #4624, #14649 ) ) ;
#14540 = CIRCLE ( 'NONE', #13866, 3.224098631618458999 ) ;
#14541 = ADVANCED_FACE ( 'NONE', ( #15994 ), #14358, .T. ) ;
#14542 = EDGE_LOOP ( 'NONE', ( #14441, #7329, #15772, #14712 ) ) ;
#14543 = ORIENTED_EDGE ( 'NONE', *, *, #15519, .F. ) ;
#14544 = EDGE_LOOP ( 'NONE', ( #653, #18207, #16602, #8943 ) ) ;
#14545 = ADVANCED_FACE ( 'NONE', ( #13103 ), #6690, .F. ) ;
#14546 = CARTESIAN_POINT ( 'NONE',  ( -28.06281046684226155, 73.06915264522029929, 248.9926560891072143 ) ) ;
#14547 = CARTESIAN_POINT ( 'NONE',  ( -139.9266654873503626, 54.05438215086714848, 31.54788804351212761 ) ) ;
#14548 = ORIENTED_EDGE ( 'NONE', *, *, #12105, .T. ) ;
#14549 = EDGE_CURVE ( 'NONE', #5714, #16297, #14253, .T. ) ;
#14550 = AXIS2_PLACEMENT_3D ( 'NONE', #14218, #6354, #12573 ) ;
#14551 = CYLINDRICAL_SURFACE ( 'NONE', #5739, 3.224098631618460331 ) ;
#14552 = CARTESIAN_POINT ( 'NONE',  ( 0.000000000000000000, 0.000000000000000000, 283.5832628385307999 ) ) ;
#14553 = CARTESIAN_POINT ( 'NONE',  ( -102.7654166546896732, -126.4532151214411755, 1.186365931940917440 ) ) ;
#14554 = ORIENTED_EDGE ( 'NONE', *, *, #7603, .F. ) ;
#14555 = VECTOR ( 'NONE', #17734, 1000.000000000000000 ) ;
#14557 = B_SPLINE_CURVE_WITH_KNOTS ( 'NONE', 3,
 ( #17827, #11575, #13192, #19713, #14451, #3705, #11924, #9641 ),
 .UNSPECIFIED., .F., .F.,
 ( 4, 2, 2, 4 ),
 ( 0.005257893453559881955, 0.006567392922673219967, 0.007876892391786557979, 0.01049589133001323747 ),
 .UNSPECIFIED. ) ;
#14556 = FACE_OUTER_BOUND ( 'NONE', #6126, .T. ) ;
#14558 = CARTESIAN_POINT ( 'NONE',  ( -48.17797692984162694, -36.99387960884178739, 283.5832628385307999 ) ) ;
#14559 = CYLINDRICAL_SURFACE ( 'NONE', #14133, 7.500000000000007105 ) ;
#14560 = DIRECTION ( 'NONE',  ( -0.2225209339563185562, 0.9749279121818227312, 0.000000000000000000 ) ) ;
#14561 = CARTESIAN_POINT ( 'NONE',  ( -27.53920554013687649, -73.25972925305620720, 248.9926560891072143 ) ) ;
#14562 = DIRECTION ( 'NONE',  ( 0.000000000000000000, 0.000000000000000000, -1.000000000000000000 ) ) ;
#14563 = ORIENTED_EDGE ( 'NONE', *, *, #19701, .T. ) ;
#14564 = PRODUCT_DEFINITION_SHAPE ( 'NONE', 'NONE',  #20248 ) ;
#14565 = CARTESIAN_POINT ( 'NONE',  ( -30.25670013172253192, -55.16472960512360402, 132.4711112102474146 ) ) ;
#14566 = VERTEX_POINT ( 'NONE', #12710 ) ;
#14567 = ORIENTED_EDGE ( 'NONE', *, *, #12485, .F. ) ;
#14568 = VERTEX_POINT ( 'NONE', #1983 ) ;
#14569 = CARTESIAN_POINT ( 'NONE',  ( 60.47951622432751151, 49.67518383744852883, 132.4711112102474146 ) ) ;
#14570 = AXIS2_PLACEMENT_3D ( 'NONE', #13449, #10167, #14768 ) ;
#14571 = CARTESIAN_POINT ( 'NONE',  ( -71.18887634719365565, -147.8252249328922687, 49.99999999999999289 ) ) ;
#14572 = DIRECTION ( 'NONE',  ( 0.6155349844899715706, -0.7881095627315598540, 0.000000000000000000 ) ) ;
#14573 = CARTESIAN_POINT ( 'NONE',  ( 27.53920554013639688, 73.25972925305639194, 248.9926560891072143 ) ) ;
#14574 = LINE ( 'NONE', #12730, #11087 ) ;
#14575 = EDGE_LOOP ( 'NONE', ( #14093, #10007, #14185, #8718 ) ) ;
#14576 = CIRCLE ( 'NONE', #533, 106.4288957539801004 ) ;
#14577 = DIRECTION ( 'NONE',  ( 0.000000000000000000, 0.000000000000000000, 1.000000000000000000 ) ) ;
#14578 = CARTESIAN_POINT ( 'NONE',  ( -2.629322876227788264, -60.68773558783006905, 293.5832628385307999 ) ) ;
#14579 = CARTESIAN_POINT ( 'NONE',  ( 58.69016442926520938, 1.379293853802370018, 132.4711112102474146 ) ) ;
#14580 = CARTESIAN_POINT ( 'NONE',  ( -50.37374754117255549, -141.2886604036510221, 49.99999999999999289 ) ) ;
#14581 = CARTESIAN_POINT ( 'NONE',  ( -20.01059462374409037, -13.41455640552162443, 39.88498244535559678 ) ) ;
#14582 = ORIENTED_EDGE ( 'NONE', *, *, #3980, .F. ) ;
#14583 = CIRCLE ( 'NONE', #12602, 62.91752772691707207 ) ;
#14584 = ORIENTED_EDGE ( 'NONE', *, *, #4270, .F. ) ;
#14585 = ORIENTED_EDGE ( 'NONE', *, *, #15036, .F. ) ;
#14586 = VERTEX_POINT ( 'NONE', #8209 ) ;
#14587 = ORIENTED_EDGE ( 'NONE', *, *, #17892, .T. ) ;
#14588 = EDGE_CURVE ( 'NONE', #16332, #11184, #17126, .T. ) ;
#14589 = AXIS2_PLACEMENT_3D ( 'NONE', #5086, #15922, #5187 ) ;
#14590 = ORIENTED_EDGE ( 'NONE', *, *, #19867, .T. ) ;
#14591 = DIRECTION ( 'NONE',  ( 0.000000000000000000, 0.000000000000000000, 1.000000000000000000 ) ) ;
#14592 = CARTESIAN_POINT ( 'NONE',  ( -56.12662799072088404, 23.22641211976270625, 293.5832628385307999 ) ) ;
#14593 = DIRECTION ( 'NONE',  ( 0.8660254037844328234, 0.5000000000000101030, 0.000000000000000000 ) ) ;
#14594 = EDGE_LOOP ( 'NONE', ( #6722, #4557, #9045, #18060 ) ) ;
#14595 = CARTESIAN_POINT ( 'NONE',  ( 54.86954475316255042, -20.84572577951183092, 248.9926560891072143 ) ) ;
#14596 = DIRECTION ( 'NONE',  ( 6.982962677686266711E-15, -0.000000000000000000, 1.000000000000000000 ) ) ;
#14597 = CIRCLE ( 'NONE', #4131, 9.000000000000000000 ) ;
#14598 = EDGE_LOOP ( 'NONE', ( #8567, #4045, #18011, #16484 ) ) ;
#14599 = AXIS2_PLACEMENT_3D ( 'NONE', #16779, #20242, #6253 ) ;
#14600 = EDGE_CURVE ( 'NONE', #9791, #17054, #14454, .T. ) ;
#14601 = LINE ( 'NONE', #11622, #11637 ) ;
#14602 = DIRECTION ( 'NONE',  ( 1.000000000000000000, 0.000000000000000000, 0.000000000000000000 ) ) ;
#14603 = CARTESIAN_POINT ( 'NONE',  ( 0.000000000000000000, 0.000000000000000000, -120.0000000000000142 ) ) ;
#14604 = ADVANCED_FACE ( 'NONE', ( #5159 ), #1775, .F. ) ;
#14605 = LINE ( 'NONE', #2606, #15180 ) ;
#14606 = AXIS2_PLACEMENT_3D ( 'NONE', #2677, #10742, #18221 ) ;
#14607 = CARTESIAN_POINT ( 'NONE',  ( 7.350000000000000533, 9.000000000000000000, 0.000000000000000000 ) ) ;
#14608 = CARTESIAN_POINT ( 'NONE',  ( 0.000000000000000000, 0.000000000000000000, 40.00000000000000000 ) ) ;
#14609 = CARTESIAN_POINT ( 'NONE',  ( 90.67862352884074539, -119.4897427140443966, 46.86044588094818408 ) ) ;
#14610 = ORIENTED_EDGE ( 'NONE', *, *, #5611, .T. ) ;
#14611 = DIRECTION ( 'NONE',  ( 1.000000000000000000, 0.000000000000000000, 0.000000000000000000 ) ) ;
#14612 = VERTEX_POINT ( 'NONE', #17439 ) ;
#14613 = ORIENTED_EDGE ( 'NONE', *, *, #12717, .F. ) ;
#14614 = ADVANCED_FACE ( 'NONE', ( #9645 ), #1873, .T. ) ;
#14615 = LINE ( 'NONE', #19328, #19390 ) ;
#14616 = ORIENTED_EDGE ( 'NONE', *, *, #2510, .T. ) ;
#14617 = LINE ( 'NONE', #12779, #1588 ) ;
#14618 = CIRCLE ( 'NONE', #1215, 32.50000000000000000 ) ;
#14619 = DIRECTION ( 'NONE',  ( -0.000000000000000000, -0.000000000000000000, -1.000000000000000000 ) ) ;
#14620 = VECTOR ( 'NONE', #6190, 1000.000000000000114 ) ;
#14621 = CARTESIAN_POINT ( 'NONE',  ( -110.0000000000000142, 285.0000000000000568, -75.00000000000000000 ) ) ;
#14622 = DIRECTION ( 'NONE',  ( -0.000000000000000000, -1.000000000000000000, -0.000000000000000000 ) ) ;
#14623 = EDGE_CURVE ( 'NONE', #13232, #1945, #4201, .T. ) ;
#14624 = CARTESIAN_POINT ( 'NONE',  ( 0.000000000000000000, 0.000000000000000000, 293.5832628385307999 ) ) ;
#14625 = CARTESIAN_POINT ( 'NONE',  ( 0.000000000000000000, 0.000000000000000000, 283.5832628385307999 ) ) ;
#14626 = CARTESIAN_POINT ( 'NONE',  ( -10.11498556985118746, 62.09913334491134407, 293.5832628385307999 ) ) ;
#14627 = ADVANCED_FACE ( 'NONE', ( #3903 ), #8899, .F. ) ;
#14628 = CARTESIAN_POINT ( 'NONE',  ( 8.939227532413712041, -60.08331549348429235, 293.5832628385307999 ) ) ;
#14629 = CYLINDRICAL_SURFACE ( 'NONE', #12178, 7.500000000000007105 ) ;
#14630 = CYLINDRICAL_SURFACE ( 'NONE', #9054, 3.224098631618460331 ) ;
#14631 = CYLINDRICAL_SURFACE ( 'NONE', #6881, 62.91752772691707207 ) ;
#14632 = CARTESIAN_POINT ( 'NONE',  ( -82.03124999999998579, -125.5821405433014064, 10.00000000000000178 ) ) ;
#14633 = AXIS2_PLACEMENT_3D ( 'NONE', #7540, #20020, #16750 ) ;
#14634 = ORIENTED_EDGE ( 'NONE', *, *, #15234, .F. ) ;
#14635 = CIRCLE ( 'NONE', #13308, 7.500000000000007105 ) ;
#14636 = CARTESIAN_POINT ( 'NONE',  ( 62.18629025319814474, -9.564549117045300974, 132.4711112102474146 ) ) ;
#14637 = CARTESIAN_POINT ( 'NONE',  ( -5.693982670708919613, 0.7000608949449669272, 283.5832628385307999 ) ) ;
#14638 = ORIENTED_EDGE ( 'NONE', *, *, #16313, .T. ) ;
#14639 = ORIENTED_EDGE ( 'NONE', *, *, #2050, .T. ) ;
#14640 = EDGE_LOOP ( 'NONE', ( #16868, #9977, #11491, #10593 ) ) ;
#14641 = EDGE_CURVE ( 'NONE', #1866, #7218, #19749, .T. ) ;
#14642 = APPLICATION_PROTOCOL_DEFINITION ( 'draft international standard', 'automotive_design', 1998, #3590 ) ;
#14643 = FACE_OUTER_BOUND ( 'NONE', #1701, .T. ) ;
#14644 = DIRECTION ( 'NONE',  ( -0.3420201433256694901, 0.9396926207859082059, 0.000000000000000000 ) ) ;
#14645 = ORIENTED_EDGE ( 'NONE', *, *, #10704, .F. ) ;
#14646 = CARTESIAN_POINT ( 'NONE',  ( -47.29944656917786006, -41.48948842197101783, 248.9926560891072143 ) ) ;
#14647 = CARTESIAN_POINT ( 'NONE',  ( -25.99419088092141550, 73.82206860051556419, 248.9926560891072143 ) ) ;
#14648 = CARTESIAN_POINT ( 'NONE',  ( -96.87131796860795419, -115.7364764686971625, 10.33971351605897304 ) ) ;
#14649 = ORIENTED_EDGE ( 'NONE', *, *, #17699, .F. ) ;
#14650 = VECTOR ( 'NONE', #1586, 1000.000000000000114 ) ;
#14651 = CIRCLE ( 'NONE', #18930, 15.91767397667354267 ) ;
#14652 = EDGE_CURVE ( 'NONE', #17581, #11236, #6978, .T. ) ;
#14653 = EDGE_CURVE ( 'NONE', #19558, #7864, #3077, .T. ) ;
#14654 = DIRECTION ( 'NONE',  ( -0.000000000000000000, -0.000000000000000000, -1.000000000000000000 ) ) ;
#14655 = EDGE_CURVE ( 'NONE', #17978, #8052, #930, .T. ) ;
#14656 = DIRECTION ( 'NONE',  ( 1.000000000000000000, 0.000000000000000000, 0.000000000000000000 ) ) ;
#14657 = DIRECTION ( 'NONE',  ( 1.000000000000000000, 0.000000000000000000, 0.000000000000000000 ) ) ;
#14658 = DIRECTION ( 'NONE',  ( -0.8830229359480271656, -0.4693298356057563625, 0.000000000000000000 ) ) ;
#14659 = CARTESIAN_POINT ( 'NONE',  ( -123.3088579006944769, -85.41493018853608987, 40.34572370108148931 ) ) ;
#14660 = VERTEX_POINT ( 'NONE', #18121 ) ;
#14661 = CARTESIAN_POINT ( 'NONE',  ( 26.42151830275484770, 4.658826548058130790, 14.88498244535526815 ) ) ;
#14662 = AXIS2_PLACEMENT_3D ( 'NONE', #12547, #18809, #9488 ) ;
#14663 = AXIS2_PLACEMENT_3D ( 'NONE', #10932, #9511, #15548 ) ;
#14664 = AXIS2_PLACEMENT_3D ( 'NONE', #2651, #1096, #15114 ) ;
#14665 = CIRCLE ( 'NONE', #4878, 62.91752772691707207 ) ;
#14666 = ORIENTED_EDGE ( 'NONE', *, *, #2753, .F. ) ;
#14667 = VERTEX_POINT ( 'NONE', #11673 ) ;
#14668 = ORIENTED_EDGE ( 'NONE', *, *, #8998, .F. ) ;
#14669 = DIRECTION ( 'NONE',  ( 1.000000000000000000, 0.000000000000000000, 0.000000000000000000 ) ) ;
#14670 = CARTESIAN_POINT ( 'NONE',  ( -127.8482905096655315, -78.45565238711304801, -8.397827111051714866 ) ) ;
#14671 = FACE_OUTER_BOUND ( 'NONE', #4717, .T. ) ;
#14672 = ADVANCED_FACE ( 'NONE', ( #17934 ), #13294, .F. ) ;
#14673 = CARTESIAN_POINT ( 'NONE',  ( 42.50000000000000000, 0.000000000000000000, -120.0000000000000142 ) ) ;
#14674 = VECTOR ( 'NONE', #13057, 999.9999999999998863 ) ;
#14675 = AXIS2_PLACEMENT_3D ( 'NONE', #14302, #12953, #5202 ) ;
#14676 = CARTESIAN_POINT ( 'NONE',  ( -3.221721112346448201, 26.95290724009910832, 39.88498244535547599 ) ) ;
#14677 = CARTESIAN_POINT ( 'NONE',  ( -125.5756761630928366, -82.07265954314213730, -1.047228856968852817 ) ) ;
#14678 = CIRCLE ( 'NONE', #6195, 3.224098631618460775 ) ;
#14679 = CARTESIAN_POINT ( 'NONE',  ( 133.2712073787624547, -68.96827650412444655, 8.924580230359330457 ) ) ;
#14680 = DIRECTION ( 'NONE',  ( 1.000000000000000000, 0.000000000000000000, 0.000000000000000000 ) ) ;
#14681 = DIRECTION ( 'NONE',  ( -0.000000000000000000, -0.000000000000000000, 1.000000000000000000 ) ) ;
#14682 = CARTESIAN_POINT ( 'NONE',  ( 0.000000000000000000, 0.000000000000000000, 248.9926560891072143 ) ) ;
#14683 = EDGE_CURVE ( 'NONE', #13051, #10874, #19462, .T. ) ;
#14684 = EDGE_LOOP ( 'NONE', ( #2941, #205 ) ) ;
#14685 = VERTEX_POINT ( 'NONE', #8515 ) ;
#14686 = ORIENTED_EDGE ( 'NONE', *, *, #16637, .F. ) ;
#14687 = AXIS2_PLACEMENT_3D ( 'NONE', #5340, #6875, #820 ) ;
#14688 = CIRCLE ( 'NONE', #5871, 65.74260934110282051 ) ;
#14689 = ORIENTED_EDGE ( 'NONE', *, *, #9380, .T. ) ;
#14690 = ORIENTED_EDGE ( 'NONE', *, *, #19854, .F. ) ;
#14691 = PLANE ( 'NONE',  #6967 ) ;
#14692 = PLANE ( 'NONE',  #6698 ) ;
#14693 = DIRECTION ( 'NONE',  ( 0.000000000000000000, 0.000000000000000000, -1.000000000000000000 ) ) ;
#14694 = ORIENTED_EDGE ( 'NONE', *, *, #5733, .F. ) ;
#14695 = CARTESIAN_POINT ( 'NONE',  ( -8.938941455414980197, 60.08127757648381362, 283.5832628385307999 ) ) ;
#14696 = FACE_OUTER_BOUND ( 'NONE', #12232, .T. ) ;
#14697 = VERTEX_POINT ( 'NONE', #13601 ) ;
#14698 = DIRECTION ( 'NONE',  ( -0.000000000000000000, -0.000000000000000000, 1.000000000000000000 ) ) ;
#14699 = FACE_OUTER_BOUND ( 'NONE', #19914, .T. ) ;
#14700 = CARTESIAN_POINT ( 'NONE',  ( 0.000000000000000000, 0.000000000000000000, 248.9926560891072143 ) ) ;
#14701 = CARTESIAN_POINT ( 'NONE',  ( -38.78191089773041256, 44.07268132743711675, 132.4711112102474146 ) ) ;
#14702 = FACE_OUTER_BOUND ( 'NONE', #15058, .T. ) ;
#14703 = DIRECTION ( 'NONE',  ( 0.9396926207859057634, -0.3420201433256758183, -6.456589605409169860E-15 ) ) ;
#14704 = FACE_OUTER_BOUND ( 'NONE', #10617, .T. ) ;
#14705 = ORIENTED_EDGE ( 'NONE', *, *, #12852, .T. ) ;
#14706 = PLANE ( 'NONE',  #3397 ) ;
#14707 = EDGE_LOOP ( 'NONE', ( #7380, #7074 ) ) ;
#14708 = EDGE_LOOP ( 'NONE', ( #1377, #11263, #14445 ) ) ;
#14709 = AXIS2_PLACEMENT_3D ( 'NONE', #1827, #15947, #291 ) ;
#14710 = DIRECTION ( 'NONE',  ( 1.000000000000000000, 0.000000000000000000, 0.000000000000000000 ) ) ;
#14711 = ORIENTED_EDGE ( 'NONE', *, *, #4227, .T. ) ;
#14712 = ORIENTED_EDGE ( 'NONE', *, *, #9209, .T. ) ;
#14713 = AXIS2_PLACEMENT_3D ( 'NONE', #5254, #17731, #8514 ) ;
#14714 = CARTESIAN_POINT ( 'NONE',  ( -110.0000000000000142, 275.0000000000000000, -75.00000000000000000 ) ) ;
#14715 = CARTESIAN_POINT ( 'NONE',  ( -98.63424005417270735, -113.0189783045208571, 49.90251308629520111 ) ) ;
#14716 = CARTESIAN_POINT ( 'NONE',  ( 48.09719419928514128, 107.5784105627835174, 39.88498244535512072 ) ) ;
#14717 = CARTESIAN_POINT ( 'NONE',  ( 1.396592535537253342E-14, 0.000000000000000000, 43.88498244535545467 ) ) ;
#14718 = EDGE_LOOP ( 'NONE', ( #19984, #13418, #15209 ) ) ;
#14719 = DIRECTION ( 'NONE',  ( -0.000000000000000000, -0.000000000000000000, 1.000000000000000000 ) ) ;
#14720 = DIRECTION ( 'NONE',  ( -0.000000000000000000, -0.000000000000000000, 1.000000000000000000 ) ) ;
#14721 = ADVANCED_FACE ( 'NONE', ( #15047 ), #10329, .T. ) ;
#14722 = LINE ( 'NONE', #14528, #13741 ) ;
#14723 = FACE_OUTER_BOUND ( 'NONE', #624, .T. ) ;
#14724 = AXIS2_PLACEMENT_3D ( 'NONE', #11333, #17589, #2033 ) ;
#14725 = ORIENTED_EDGE ( 'NONE', *, *, #5310, .T. ) ;
#14726 = CYLINDRICAL_SURFACE ( 'NONE', #4326, 7.500000000000007105 ) ;
#14727 = CARTESIAN_POINT ( 'NONE',  ( -60.08127757648377099, -8.938941455415186255, 293.5832628385307999 ) ) ;
#14728 = DIRECTION ( 'NONE',  ( -0.000000000000000000, -0.000000000000000000, -1.000000000000000000 ) ) ;
#14729 = AXIS2_PLACEMENT_3D ( 'NONE', #15509, #4773, #17252 ) ;
#14730 = DIRECTION ( 'NONE',  ( -0.7660444431189857850, -0.6427876096865299260, 5.349259755748838558E-15 ) ) ;
#14731 = ORIENTED_EDGE ( 'NONE', *, *, #18119, .F. ) ;
#14732 = LINE ( 'NONE', #18105, #13981 ) ;
#14733 = DIRECTION ( 'NONE',  ( 1.000000000000000000, 0.000000000000000000, 0.000000000000000000 ) ) ;
#14734 = ORIENTED_EDGE ( 'NONE', *, *, #1997, .F. ) ;
#14735 = EDGE_LOOP ( 'NONE', ( #8236, #2850, #5139, #10108 ) ) ;
#14736 = B_SPLINE_CURVE_WITH_KNOTS ( 'NONE', 3,
 ( #9517, #12977, #19235, #5222, #17705, #2151, #3281, #17303 ),
 .UNSPECIFIED., .F., .F.,
 ( 4, 2, 2, 4 ),
 ( 0.005257893453559887159, 0.006567392922673222569, 0.007876892391786557979, 0.01049589133001322533 ),
 .UNSPECIFIED. ) ;
#14737 = CONTEXT_DEPENDENT_SHAPE_REPRESENTATION ( #14812, #2944 ) ;
#14738 = ADVANCED_FACE ( 'NONE', ( #7079 ), #19847, .T. ) ;
#14739 = EDGE_CURVE ( 'NONE', #6064, #6223, #1777, .T. ) ;
#14740 = EDGE_LOOP ( 'NONE', ( #9934, #7294, #18399, #12550 ) ) ;
#14741 = ADVANCED_FACE ( 'NONE', ( #5543 ), #1026, .F. ) ;
#14742 = LINE ( 'NONE', #722, #14362 ) ;
#14743 = LINE ( 'NONE', #1020, #9371 ) ;
#14744 = ORIENTED_EDGE ( 'NONE', *, *, #5915, .T. ) ;
#14745 = AXIS2_PLACEMENT_3D ( 'NONE', #16714, #19484, #13423 ) ;
#14746 = CARTESIAN_POINT ( 'NONE',  ( 96.05623471150424564, -115.3294058443303669, 4.799833099651143797 ) ) ;
#14747 = FACE_BOUND ( 'NONE', #15571, .T. ) ;
#14748 = CARTESIAN_POINT ( 'NONE',  ( -97.93656923779387569, -133.3799209237830041, 7.071677858121607763 ) ) ;
#14749 = EDGE_CURVE ( 'NONE', #3424, #7495, #10051, .T. ) ;
#14750 = CARTESIAN_POINT ( 'NONE',  ( -83.21341172527399976, -124.8022162803316348, 2.974423032988927407 ) ) ;
#14751 = CARTESIAN_POINT ( 'NONE',  ( -82.43884259638412004, -58.61746404108814801, 14.88498244535602844 ) ) ;
#14752 = DIRECTION ( 'NONE',  ( 0.9848077530122080203, 0.1736481776669307198, 0.000000000000000000 ) ) ;
#14753 = DIRECTION ( 'NONE',  ( 0.000000000000000000, 0.000000000000000000, 1.000000000000000000 ) ) ;
#14754 = CARTESIAN_POINT ( 'NONE',  ( 105.9946577255055331, 51.49356311920430329, 39.88498244535471571 ) ) ;
#14755 = VERTEX_POINT ( 'NONE', #13197 ) ;
#14756 = CYLINDRICAL_SURFACE ( 'NONE', #5811, 3.224098631618460331 ) ;
#14757 = CARTESIAN_POINT ( 'NONE',  ( -17.24542129382122724, 20.55229278271246329, 14.88498244535557369 ) ) ;
#14758 = EDGE_CURVE ( 'NONE', #3694, #5829, #18029, .T. ) ;
#14759 = ORIENTED_EDGE ( 'NONE', *, *, #15623, .T. ) ;
#14760 = ADVANCED_FACE ( 'NONE', ( #14939 ), #13498, .F. ) ;
#14761 = PRODUCT_RELATED_PRODUCT_CATEGORY ( 'part', '', ( #4 ) ) ;
#14762 = EDGE_LOOP ( 'NONE', ( #9332, #12215, #12283, #3839 ) ) ;
#14763 = DIRECTION ( 'NONE',  ( -0.000000000000000000, -0.000000000000000000, 1.000000000000000000 ) ) ;
#14764 = CARTESIAN_POINT ( 'NONE',  ( -130.7934332354521132, -73.44669674648567081, -5.542612327196102306 ) ) ;
#14765 = CARTESIAN_POINT ( 'NONE',  ( 1.396592535537252080E-14, 0.000000000000000000, 43.88498244535546178 ) ) ;
#14766 = CARTESIAN_POINT ( 'NONE',  ( -60.00000000000000000, -2.094888803305880013E-13, -100.0000000000000000 ) ) ;
#14767 = DIRECTION ( 'NONE',  ( -0.7881095627315599650, -0.6155349844899714595, 0.000000000000000000 ) ) ;
#14768 = DIRECTION ( 'NONE',  ( 1.000000000000000000, 0.000000000000000000, 0.000000000000000000 ) ) ;
#14769 = EDGE_CURVE ( 'NONE', #11267, #17576, #19735, .T. ) ;
#14770 = CARTESIAN_POINT ( 'NONE',  ( 134.6257061167716813, -73.66332987389617415, 7.420084151274023654 ) ) ;
#14771 = VECTOR ( 'NONE', #11487, 1000.000000000000000 ) ;
#14772 = AXIS2_PLACEMENT_3D ( 'NONE', #1387, #7721, #4452 ) ;
#14773 = FACE_OUTER_BOUND ( 'NONE', #18754, .T. ) ;
#14774 = LINE ( 'NONE', #10359, #17572 ) ;
#14775 = VERTEX_POINT ( 'NONE', #7775 ) ;
#14776 = CIRCLE ( 'NONE', #13797, 7.500000000000003553 ) ;
#14777 = VECTOR ( 'NONE', #16790, 1000.000000000000227 ) ;
#14778 = EDGE_LOOP ( 'NONE', ( #11440, #11092 ) ) ;
#14779 = ORIENTED_EDGE ( 'NONE', *, *, #1724, .T. ) ;
#14780 = ADVANCED_FACE ( 'NONE', ( #9207, #13706, #18525, #1545, #4613, #16889, #10836, #12273 ), #1229, .T. ) ;
#14781 = ORIENTED_EDGE ( 'NONE', *, *, #13876, .T. ) ;
#14782 = PLANE ( 'NONE',  #13490 ) ;
#14783 = AXIS2_PLACEMENT_3D ( 'NONE', #9726, #6674, #5143 ) ;
#14784 = AXIS2_PLACEMENT_3D ( 'NONE', #16589, #12274, #15144 ) ;
#14785 = ORIENTED_EDGE ( 'NONE', *, *, #6031, .T. ) ;
#14786 = EDGE_CURVE ( 'NONE', #20169, #4629, #14017, .T. ) ;
#14787 = DIRECTION ( 'NONE',  ( 1.000000000000000000, 0.000000000000000000, 0.000000000000000000 ) ) ;
#14788 = DIRECTION ( 'NONE',  ( -0.4999999999999889533, -0.8660254037844450359, 0.000000000000000000 ) ) ;
#14789 = DIRECTION ( 'NONE',  ( 0.5000000000000101030, -0.8660254037844328234, 0.000000000000000000 ) ) ;
#14790 = ORIENTED_EDGE ( 'NONE', *, *, #17857, .T. ) ;
#14791 = EDGE_CURVE ( 'NONE', #13413, #807, #7648, .T. ) ;
#14792 = VECTOR ( 'NONE', #10296, 1000.000000000000227 ) ;
#14793 = LINE ( 'NONE', #16240, #14877 ) ;
#14794 = FACE_OUTER_BOUND ( 'NONE', #5016, .T. ) ;
#14795 = VERTEX_POINT ( 'NONE', #18736 ) ;
#14796 = LINE ( 'NONE', #8655, #940 ) ;
#14797 = CARTESIAN_POINT ( 'NONE',  ( -39.80940113485986842, 48.72193424476489554, 293.5832628385307999 ) ) ;
#14798 = LINE ( 'NONE', #8459, #6191 ) ;
#14799 = CARTESIAN_POINT ( 'NONE',  ( 0.000000000000000000, 0.000000000000000000, 283.5832628385307999 ) ) ;
#14800 = VECTOR ( 'NONE', #6343, 1000.000000000000000 ) ;
#14801 = VECTOR ( 'NONE', #4740, 1000.000000000000114 ) ;
#14802 = CARTESIAN_POINT ( 'NONE',  ( -54.07248341783231638, 32.16802499836798290, 293.5832628385307999 ) ) ;
#14803 = CARTESIAN_POINT ( 'NONE',  ( -39.37628763770455009, -49.07263256785938665, 293.5832628385307999 ) ) ;
#14804 = CARTESIAN_POINT ( 'NONE',  ( 68.18670162478805707, 38.41834839689404646, 110.9660488491356887 ) ) ;
#14805 = ORIENTED_EDGE ( 'NONE', *, *, #7705, .T. ) ;
#14806 = CARTESIAN_POINT ( 'NONE',  ( 47.29944656917757584, 41.48948842197132336, 293.5832628385307999 ) ) ;
#14807 = VERTEX_POINT ( 'NONE', #12061 ) ;
#14808 = CIRCLE ( 'NONE', #6664, 7.500000000000007105 ) ;
#14809 = EDGE_LOOP ( 'NONE', ( #11679, #19687, #11004, #16182, #10497 ) ) ;
#14810 = FACE_OUTER_BOUND ( 'NONE', #558, .T. ) ;
#14811 = AXIS2_PLACEMENT_3D ( 'NONE', #5945, #7768, #7562 ) ;
#14812 =( REPRESENTATION_RELATIONSHIP ('NONE','NONE', #17382, #15821 ) REPRESENTATION_RELATIONSHIP_WITH_TRANSFORMATION ( #8499 )SHAPE_REPRESENTATION_RELATIONSHIP( ) );
#14813 = ORIENTED_EDGE ( 'NONE', *, *, #18242, .F. ) ;
#14814 = DIRECTION ( 'NONE',  ( -6.982962677686266711E-15, 0.000000000000000000, -1.000000000000000000 ) ) ;
#14815 = VECTOR ( 'NONE', #13157, 1000.000000000000000 ) ;
#14816 = FACE_OUTER_BOUND ( 'NONE', #11058, .T. ) ;
#14817 = CARTESIAN_POINT ( 'NONE',  ( 60.08331549348424971, 8.939227532413909216, 283.5832628385307999 ) ) ;
#14818 = VERTEX_POINT ( 'NONE', #2777 ) ;
#14819 = LINE ( 'NONE', #11830, #17858 ) ;
#14820 = LINE ( 'NONE', #17805, #7140 ) ;
#14821 = VECTOR ( 'NONE', #3819, 999.9999999999998863 ) ;
#14822 = CARTESIAN_POINT ( 'NONE',  ( 25.99419088092191643, -73.82206860051539365, 111.4180192758973362 ) ) ;
#14823 = DIRECTION ( 'NONE',  ( 0.000000000000000000, 0.000000000000000000, 1.000000000000000000 ) ) ;
#14824 = LINE ( 'NONE', #712, #19372 ) ;
#14825 = AXIS2_PLACEMENT_3D ( 'NONE', #17704, #19712, #17996 ) ;
#14826 = CARTESIAN_POINT ( 'NONE',  ( -78.85162031257850401, -85.37653928070189124, 14.88498244535600357 ) ) ;
#14827 = CARTESIAN_POINT ( 'NONE',  ( 58.69016442926523069, -0.8220851292429179891, 132.4711112102474146 ) ) ;
#14828 = DIRECTION ( 'NONE',  ( 0.9009688679024152602, 0.4338837391175662805, -0.000000000000000000 ) ) ;
#14829 = ORIENTED_EDGE ( 'NONE', *, *, #11626, .F. ) ;
#14830 = CARTESIAN_POINT ( 'NONE',  ( 156.4179374840099683, -52.02840013023883614, 39.99999999999999289 ) ) ;
#14831 = CYLINDRICAL_SURFACE ( 'NONE', #12190, 106.4288957539801004 ) ;
#14832 = ORIENTED_EDGE ( 'NONE', *, *, #17165, .F. ) ;
#14833 = ORIENTED_EDGE ( 'NONE', *, *, #3226, .T. ) ;
#14834 = AXIS2_PLACEMENT_3D ( 'NONE', #12704, #13932, #18658 ) ;
#14835 = EDGE_CURVE ( 'NONE', #2991, #10778, #15166, .T. ) ;
#14836 = DIRECTION ( 'NONE',  ( -6.982962677686266711E-15, 0.000000000000000000, -1.000000000000000000 ) ) ;
#14837 = AXIS2_PLACEMENT_3D ( 'NONE', #458, #11400, #10066 ) ;
#14838 = EDGE_LOOP ( 'NONE', ( #9179, #6580 ) ) ;
#14839 = CARTESIAN_POINT ( 'NONE',  ( 87.56486837567058501, -121.7886324248894141, -4.190568952157736504 ) ) ;
#14840 = CARTESIAN_POINT ( 'NONE',  ( -95.87737486567888823, -116.0928213521003869, 9.446122864778402572 ) ) ;
#14841 = ORIENTED_EDGE ( 'NONE', *, *, #2526, .F. ) ;
#14842 = CARTESIAN_POINT ( 'NONE',  ( -82.03124999999998579, -125.5821405433014064, 10.00000000000000178 ) ) ;
#14843 = DIRECTION ( 'NONE',  ( 1.000000000000000000, 0.000000000000000000, 0.000000000000000000 ) ) ;
#14844 = ADVANCED_FACE ( 'NONE', ( #18325 ), #6261, .F. ) ;
#14845 = CARTESIAN_POINT ( 'NONE',  ( -25.99419088092141550, 73.82206860051556419, 132.4711112102474146 ) ) ;
#14846 = AXIS2_PLACEMENT_3D ( 'NONE', #19047, #1956, #8184 ) ;
#14847 = DIRECTION ( 'NONE',  ( 1.000000000000000000, 0.000000000000000000, 0.000000000000000000 ) ) ;
#14848 = CARTESIAN_POINT ( 'NONE',  ( 0.000000000000000000, 0.000000000000000000, 283.5832628385307999 ) ) ;
#14849 = EDGE_LOOP ( 'NONE', ( #17057, #7324, #10135, #17453 ) ) ;
#14850 = EDGE_CURVE ( 'NONE', #3096, #6110, #13810, .T. ) ;
#14851 = DIRECTION ( 'NONE',  ( -0.9848077530122104628, 0.1736481776669172861, 0.000000000000000000 ) ) ;
#14852 = CARTESIAN_POINT ( 'NONE',  ( -144.1130761623740568, -69.50842595698578918, 30.00000000000000000 ) ) ;
#14853 = VERTEX_POINT ( 'NONE', #1442 ) ;
#14854 = MANIFOLD_SOLID_BREP ( 'Boss-Extrude11', #10013 ) ;
#14855 = CIRCLE ( 'NONE', #14550, 60.74260934110282051 ) ;
#14856 = EDGE_LOOP ( 'NONE', ( #6248, #11488, #1835 ) ) ;
#14857 = EDGE_CURVE ( 'NONE', #13590, #10563, #20056, .T. ) ;
#14858 = CARTESIAN_POINT ( 'NONE',  ( -176.7850001792984926, -188.8278678429259685, 7.673622252739133565 ) ) ;
#14859 = ORIENTED_EDGE ( 'NONE', *, *, #14424, .F. ) ;
#14860 = AXIS2_PLACEMENT_3D ( 'NONE', #1003, #2652, #2259 ) ;
#14861 = CARTESIAN_POINT ( 'NONE',  ( 0.000000000000000000, 0.000000000000000000, 283.5832628385307999 ) ) ;
#14862 = PLANE ( 'NONE',  #14189 ) ;
#14863 = PLANE ( 'NONE',  #14952 ) ;
#14864 = CARTESIAN_POINT ( 'NONE',  ( 73.61113626724119285, -92.47916748300480094, 14.88498244535493598 ) ) ;
#14865 = DIRECTION ( 'NONE',  ( 0.9781142164131917394, -0.2080686897406911207, 0.000000000000000000 ) ) ;
#14866 = CARTESIAN_POINT ( 'NONE',  ( -71.18887634719365565, -147.8252249328922687, 39.99999999999999289 ) ) ;
#14867 = ADVANCED_FACE ( 'NONE', ( #18636 ), #17409, .T. ) ;
#14868 = CARTESIAN_POINT ( 'NONE',  ( -5.281164089014724006, -2.240720816136035243, 293.5832628385307999 ) ) ;
#14869 = EDGE_CURVE ( 'NONE', #18649, #2503, #5061, .T. ) ;
#14870 = FACE_OUTER_BOUND ( 'NONE', #17625, .T. ) ;
#14871 = VECTOR ( 'NONE', #16364, 1000.000000000000000 ) ;
#14872 = DIRECTION ( 'NONE',  ( 0.9749279121818255067, -0.2225209339563057331, 0.000000000000000000 ) ) ;
#14873 = ADVANCED_FACE ( 'NONE', ( #15968 ), #6461, .F. ) ;
#14874 = ORIENTED_EDGE ( 'NONE', *, *, #8592, .T. ) ;
#14875 = ORIENTED_EDGE ( 'NONE', *, *, #4870, .T. ) ;
#14876 = VERTEX_POINT ( 'NONE', #309 ) ;
#14877 = VECTOR ( 'NONE', #8454, 1000.000000000000227 ) ;
#14878 = ORIENTED_EDGE ( 'NONE', *, *, #20028, .T. ) ;
#14879 = EDGE_CURVE ( 'NONE', #15471, #12923, #8643, .T. ) ;
#14880 = ORIENTED_EDGE ( 'NONE', *, *, #5665, .T. ) ;
#14881 = AXIS2_PLACEMENT_3D ( 'NONE', #15531, #18494, #13884 ) ;
#14882 = CARTESIAN_POINT ( 'NONE',  ( -68.46530598706770832, 37.93579148621532937, 132.4711112102474146 ) ) ;
#14883 = LINE ( 'NONE', #17870, #7976 ) ;
#14884 = CARTESIAN_POINT ( 'NONE',  ( -0.7000608949449798057, -5.693982670708954252, 283.5832628385307999 ) ) ;
#14885 = ORIENTED_EDGE ( 'NONE', *, *, #15915, .F. ) ;
#14886 = CARTESIAN_POINT ( 'NONE',  ( 53.40245231972179596, 28.94983032429848535, 283.5832628385307999 ) ) ;
#14887 = DIRECTION ( 'NONE',  ( 0.000000000000000000, 1.000000000000000000, 0.000000000000000000 ) ) ;
#14888 = ORIENTED_EDGE ( 'NONE', *, *, #7386, .T. ) ;
#14889 = PLANE ( 'NONE',  #18252 ) ;
#14890 = LINE ( 'NONE', #14797, #16558 ) ;
#14891 = CARTESIAN_POINT ( 'NONE',  ( -134.5351519296995662, -74.34771143809115301, 6.414883565331459536 ) ) ;
#14892 = EDGE_CURVE ( 'NONE', #17841, #19981, #2115, .T. ) ;
#14893 = EDGE_CURVE ( 'NONE', #1634, #1213, #3484, .T. ) ;
#14894 = CARTESIAN_POINT ( 'NONE',  ( 44.79940644582654841, -41.02350267428983699, 283.5832628385307999 ) ) ;
#14896 = ADVANCED_FACE ( 'NONE', ( #14529 ), #12683, .T. ) ;
#14895 = CIRCLE ( 'NONE', #2815, 9.999999999999992895 ) ;
#14897 = AXIS2_PLACEMENT_3D ( 'NONE', #1917, #15626, #11008 ) ;
#14898 = CYLINDRICAL_SURFACE ( 'NONE', #14940, 7.500000000000002665 ) ;
#14899 = DIRECTION ( 'NONE',  ( -6.982962677686266711E-15, 0.000000000000000000, -1.000000000000000000 ) ) ;
#14900 = VERTEX_POINT ( 'NONE', #14433 ) ;
#14901 = CIRCLE ( 'NONE', #3812, 32.50000000000000000 ) ;
#14902 = DIRECTION ( 'NONE',  ( 1.224646799147353207E-16, 1.000000000000000000, -0.000000000000000000 ) ) ;
#14903 = ORIENTED_EDGE ( 'NONE', *, *, #9526, .T. ) ;
#14904 = ORIENTED_EDGE ( 'NONE', *, *, #12257, .F. ) ;
#14905 = DIRECTION ( 'NONE',  ( -1.000000000000000000, 0.000000000000000000, 0.000000000000000000 ) ) ;
#14906 = ORIENTED_EDGE ( 'NONE', *, *, #12374, .T. ) ;
#14907 = ORIENTED_EDGE ( 'NONE', *, *, #15249, .F. ) ;
#14908 = CARTESIAN_POINT ( 'NONE',  ( 128.2779226595531270, 102.2982297021113141, 49.99999999999999289 ) ) ;
#14909 = VECTOR ( 'NONE', #6427, 1000.000000000000227 ) ;
#14910 = B_SPLINE_CURVE_WITH_KNOTS ( 'NONE', 3,
 ( #7518, #2721, #1172, #1594, #15400, #7418, #10791, #1386, #2825, #4561, #10682, #10477, #13653, #17147, #17046, #12220, #16939, #3031, #13755, #56, #20204, #15506, #16732, #1492, #6209, #13960, #18688, #12426, #19900, #7824 ),
 .UNSPECIFIED., .F., .F.,
 ( 4, 2, 2, 2, 2, 2, 2, 2, 2, 2, 2, 2, 2, 2, 4 ),
 ( 2.251336500357276218E-07, 0.003672487653379172701, 0.007344750173108309521, 0.009180881432972864270, 0.01101701269283741902, 0.01468927521256654586, 0.02203380025202480302, 0.02386993151188936471, 0.02570606277175392293, 0.02937832529148303590, 0.03672285033094124795, 0.04406737537039945307, 0.04773963789012858339, 0.05141190040985771370, 0.05875642544931597433 ),
 .UNSPECIFIED. ) ;
#14911 = CARTESIAN_POINT ( 'NONE',  ( -96.48429163929540664, -114.8598460512868940, 49.50248771032619288 ) ) ;
#14912 = FACE_OUTER_BOUND ( 'NONE', #6345, .T. ) ;
#14913 = ORIENTED_EDGE ( 'NONE', *, *, #17806, .T. ) ;
#14914 = AXIS2_PLACEMENT_3D ( 'NONE', #2263, #18101, #3976 ) ;
#14915 = CARTESIAN_POINT ( 'NONE',  ( -123.6373235125731753, -84.94667440144655757, 50.00000000000000000 ) ) ;
#14916 = DIRECTION ( 'NONE',  ( 0.5300553768524375320, 0.8479630283625697595, 0.000000000000000000 ) ) ;
#14917 = EDGE_CURVE ( 'NONE', #19299, #6975, #8952, .T. ) ;
#14918 = DIRECTION ( 'NONE',  ( 0.000000000000000000, 0.000000000000000000, -1.000000000000000000 ) ) ;
#14919 = CARTESIAN_POINT ( 'NONE',  ( 92.34802049131684498, -66.64338626758360817, 14.88498244535480630 ) ) ;
#14920 = VERTEX_POINT ( 'NONE', #15763 ) ;
#14921 = CARTESIAN_POINT ( 'NONE',  ( -115.2828271789296650, -14.71737894807794156, 14.88498244535625759 ) ) ;
#14922 = CARTESIAN_POINT ( 'NONE',  ( -15.91767397667354800, 164.0736214083062805, 60.00000000000000000 ) ) ;
#14923 = DIRECTION ( 'NONE',  ( 0.9848077530122085754, -0.1736481776669273336, 0.000000000000000000 ) ) ;
#14924 = EDGE_CURVE ( 'NONE', #1866, #12611, #6692, .T. ) ;
#14925 = ORIENTED_EDGE ( 'NONE', *, *, #6394, .F. ) ;
#14926 = LINE ( 'NONE', #14830, #15969 ) ;
#14927 = CARTESIAN_POINT ( 'NONE',  ( 22.81000261549367991, -58.63718168490493099, 248.9926560891072143 ) ) ;
#14928 = ORIENTED_EDGE ( 'NONE', *, *, #1795, .F. ) ;
#14929 = ORIENTED_EDGE ( 'NONE', *, *, #8885, .T. ) ;
#14930 = AXIS2_PLACEMENT_3D ( 'NONE', #519, #616, #6860 ) ;
#14931 = DIRECTION ( 'NONE',  ( -0.4338837391175509040, -0.9009688679024224767, 0.000000000000000000 ) ) ;
#14932 = CARTESIAN_POINT ( 'NONE',  ( -31.77296517111735596, -51.77251465595229263, 293.5832628385307999 ) ) ;
#14933 = ORIENTED_EDGE ( 'NONE', *, *, #11308, .T. ) ;
#14934 = CARTESIAN_POINT ( 'NONE',  ( 106.3851141486848064, -120.5004170265810330, 0.04616215448129540322 ) ) ;
#14935 = CARTESIAN_POINT ( 'NONE',  ( -105.2683707665257629, -122.4156632037601611, 0.2357454945587965922 ) ) ;
#14936 = AXIS2_PLACEMENT_3D ( 'NONE', #5921, #8868, #3054 ) ;
#14937 = DIRECTION ( 'NONE',  ( -0.7881095627315599650, -0.6155349844899714595, 0.000000000000000000 ) ) ;
#14938 = DIRECTION ( 'NONE',  ( 0.9848077530122073542, 0.1736481776669340227, -0.000000000000000000 ) ) ;
#14939 = FACE_OUTER_BOUND ( 'NONE', #1703, .T. ) ;
#14940 = AXIS2_PLACEMENT_3D ( 'NONE', #881, #10290, #12119 ) ;
#14941 = DIRECTION ( 'NONE',  ( -0.3088643371590125697, 0.9511061040868803440, 0.000000000000000000 ) ) ;
#14942 = AXIS2_PLACEMENT_3D ( 'NONE', #8333, #3640, #11307 ) ;
#14943 = DIRECTION ( 'NONE',  ( -0.7430374143461878633, 0.6692498792541777819, 0.000000000000000000 ) ) ;
#14944 = LINE ( 'NONE', #13401, #16428 ) ;
#14945 = LINE ( 'NONE', #19752, #15782 ) ;
#14946 = EDGE_CURVE ( 'NONE', #4516, #195, #1744, .T. ) ;
#14947 = VERTEX_POINT ( 'NONE', #9620 ) ;
#14948 = DIRECTION ( 'NONE',  ( -0.000000000000000000, -0.000000000000000000, 1.000000000000000000 ) ) ;
#14949 = DIRECTION ( 'NONE',  ( 0.000000000000000000, 1.000000000000000000, -3.338476886082577323E-16 ) ) ;
#14950 = ORIENTED_EDGE ( 'NONE', *, *, #4392, .T. ) ;
#14951 = ORIENTED_EDGE ( 'NONE', *, *, #1508, .T. ) ;
#14952 = AXIS2_PLACEMENT_3D ( 'NONE', #13028, #14572, #16213 ) ;
#14953 = VERTEX_POINT ( 'NONE', #16174 ) ;
#14954 = AXIS2_PLACEMENT_3D ( 'NONE', #1107, #20039, #6037 ) ;
#14955 = ADVANCED_FACE ( 'NONE', ( #9924 ), #3587, .T. ) ;
#14956 = CARTESIAN_POINT ( 'NONE',  ( -152.4599531637108498, -36.50981547337168109, 39.99999999999999289 ) ) ;
#14957 = EDGE_LOOP ( 'NONE', ( #3601, #5288, #18520, #13317 ) ) ;
#14958 = CARTESIAN_POINT ( 'NONE',  ( 134.6804726163186956, -73.23883837743916558, 8.316693297614211389 ) ) ;
#14959 = CARTESIAN_POINT ( 'NONE',  ( 97.50000000000002842, -189.9999999999999716, 10.00000000000000178 ) ) ;
#14960 = DIRECTION ( 'NONE',  ( -0.3427509529624101492, 0.9394263059140720573, 0.000000000000000000 ) ) ;
#14961 = LINE ( 'NONE', #16416, #7707 ) ;
#14962 = DIRECTION ( 'NONE',  ( -0.03505990758545895342, -0.9993852124581886764, 0.000000000000000000 ) ) ;
#14963 = CARTESIAN_POINT ( 'NONE',  ( -156.4179374840092862, -52.02840013024096066, 60.00000000000000000 ) ) ;
#14964 = CARTESIAN_POINT ( 'NONE',  ( -126.6692879288293341, -80.35371549668381874, -9.119744649247303769 ) ) ;
#14965 = CARTESIAN_POINT ( 'NONE',  ( 135.1060089016586119, -65.16414933584998437, 8.475570270055174049 ) ) ;
#14966 = AXIS2_PLACEMENT_3D ( 'NONE', #797, #14814, #7241 ) ;
#14967 = FACE_OUTER_BOUND ( 'NONE', #6359, .T. ) ;
#14968 = DIRECTION ( 'NONE',  ( 0.6155349844899687950, -0.7881095627315619634, 0.000000000000000000 ) ) ;
#14969 = AXIS2_PLACEMENT_3D ( 'NONE', #1326, #10515, #13694 ) ;
#14970 = CARTESIAN_POINT ( 'NONE',  ( -47.56244194535165803, -37.78198917157333625, 293.5832628385307999 ) ) ;
#14971 = CIRCLE ( 'NONE', #11063, 32.50000000000000000 ) ;
#14972 = EDGE_CURVE ( 'NONE', #12460, #4464, #1846, .T. ) ;
#14973 = ORIENTED_EDGE ( 'NONE', *, *, #9610, .F. ) ;
#14974 = AXIS2_PLACEMENT_3D ( 'NONE', #14378, #9767, #6709 ) ;
#14975 = EDGE_CURVE ( 'NONE', #2533, #15182, #13520, .T. ) ;
#14976 = ORIENTED_EDGE ( 'NONE', *, *, #5553, .F. ) ;
#14977 = EDGE_LOOP ( 'NONE', ( #4602, #15034, #9825, #5407 ) ) ;
#14978 = ORIENTED_EDGE ( 'NONE', *, *, #2251, .T. ) ;
#14979 = EDGE_CURVE ( 'NONE', #2173, #7363, #7015, .T. ) ;
#14980 = ORIENTED_EDGE ( 'NONE', *, *, #3274, .F. ) ;
#14981 = EDGE_CURVE ( 'NONE', #16297, #1477, #19244, .T. ) ;
#14982 = AXIS2_PLACEMENT_3D ( 'NONE', #9595, #286, #15538 ) ;
#14983 = AXIS2_PLACEMENT_3D ( 'NONE', #2027, #19112, #5297 ) ;
#14984 = EDGE_CURVE ( 'NONE', #3256, #8052, #2160, .T. ) ;
#14985 = AXIS2_PLACEMENT_3D ( 'NONE', #3330, #8027, #19090 ) ;
#14986 = DIRECTION ( 'NONE',  ( -0.000000000000000000, -0.000000000000000000, -1.000000000000000000 ) ) ;
#14987 = DIRECTION ( 'NONE',  ( 0.000000000000000000, 0.000000000000000000, -1.000000000000000000 ) ) ;
#14988 = ORIENTED_EDGE ( 'NONE', *, *, #19884, .T. ) ;
#14989 = CARTESIAN_POINT ( 'NONE',  ( 0.3563104543936318480, -9.539178283403844105, 1.477658550686873129 ) ) ;
#14990 = FACE_OUTER_BOUND ( 'NONE', #528, .T. ) ;
#14991 = ORIENTED_EDGE ( 'NONE', *, *, #2423, .T. ) ;
#14992 = CARTESIAN_POINT ( 'NONE',  ( 7.950000000000000178, 10.39230484541327471, 0.000000000000000000 ) ) ;
#14993 = DIRECTION ( 'NONE',  ( -0.000000000000000000, -0.000000000000000000, 1.000000000000000000 ) ) ;
#14994 = CYLINDRICAL_SURFACE ( 'NONE', #9764, 15.91767397667355510 ) ;
#14995 = CARTESIAN_POINT ( 'NONE',  ( -85.53020504959707182, -140.9188050298390067, 39.99999999999999289 ) ) ;
#14996 = EDGE_CURVE ( 'NONE', #18905, #15888, #12577, .T. ) ;
#14997 = EDGE_CURVE ( 'NONE', #6696, #3720, #12225, .T. ) ;
#14998 = DIRECTION ( 'NONE',  ( 0.6427876096865481337, -0.7660444431189707970, 0.000000000000000000 ) ) ;
#14999 = PLANE ( 'NONE',  #8697 ) ;
#15000 = AXIS2_PLACEMENT_3D ( 'NONE', #9571, #58, #20104 ) ;
#15001 = CIRCLE ( 'NONE', #12726, 39.99999999999997868 ) ;
#15002 = EDGE_LOOP ( 'NONE', ( #13016, #13229, #10325, #12694 ) ) ;
#15003 = CARTESIAN_POINT ( 'NONE',  ( 0.8038475772931082952, -5.196152422707021934, -8.999999999999998224 ) ) ;
#15004 = ORIENTED_EDGE ( 'NONE', *, *, #15262, .T. ) ;
#15005 = EDGE_LOOP ( 'NONE', ( #18067, #8179, #19095, #3270 ) ) ;
#15006 = DIRECTION ( 'NONE',  ( -0.9848077530122085754, 0.1736481776669273336, 0.000000000000000000 ) ) ;
#15007 = ORIENTED_EDGE ( 'NONE', *, *, #19996, .T. ) ;
#15008 = VERTEX_POINT ( 'NONE', #13079 ) ;
#15009 = EDGE_CURVE ( 'NONE', #11373, #2503, #12556, .T. ) ;
#15010 = EDGE_CURVE ( 'NONE', #9076, #17815, #5382, .T. ) ;
#15011 = ADVANCED_FACE ( 'NONE', ( #11835 ), #17906, .T. ) ;
#15012 = LINE ( 'NONE', #892, #16934 ) ;
#15013 = EDGE_CURVE ( 'NONE', #12045, #11852, #13272, .T. ) ;
#15014 = CARTESIAN_POINT ( 'NONE',  ( -82.03124999999998579, -125.5821405433014064, 30.00000000000000000 ) ) ;
#15015 = CARTESIAN_POINT ( 'NONE',  ( 8.938941455415006843, -60.08127757648380651, 293.5832628385307999 ) ) ;
#15016 = PLANE ( 'NONE',  #14014 ) ;
#15017 = AXIS2_PLACEMENT_3D ( 'NONE', #14766, #19870, #5767 ) ;
#15018 = EDGE_LOOP ( 'NONE', ( #3299, #19265, #14341, #18258 ) ) ;
#15019 = CARTESIAN_POINT ( 'NONE',  ( -124.4476442249722226, -83.75451619235309408, 49.87919367093176959 ) ) ;
#15020 = CARTESIAN_POINT ( 'NONE',  ( -59.42266395395758138, 50.93469132750324491, 132.4711112102474146 ) ) ;
#15021 = CARTESIAN_POINT ( 'NONE',  ( 0.8038475772933632024, 5.196152422706628471, 9.000000000000001776 ) ) ;
#15022 = CYLINDRICAL_SURFACE ( 'NONE', #14860, 106.4288957539801004 ) ;
#15023 = ORIENTED_EDGE ( 'NONE', *, *, #8219, .T. ) ;
#15024 = EDGE_CURVE ( 'NONE', #13684, #10955, #11555, .T. ) ;
#15025 = LINE ( 'NONE', #4485, #9707 ) ;
#15026 = CARTESIAN_POINT ( 'NONE',  ( -132.6218665116185491, -85.29503539049817107, 39.26870858449429846 ) ) ;
#15027 = CARTESIAN_POINT ( 'NONE',  ( 0.000000000000000000, 0.000000000000000000, 132.4711112102474146 ) ) ;
#15028 = ORIENTED_EDGE ( 'NONE', *, *, #20238, .F. ) ;
#15029 = VECTOR ( 'NONE', #17516, 1000.000000000000000 ) ;
#15030 = CARTESIAN_POINT ( 'NONE',  ( 114.2960429025576587, -28.68569479505797659, 14.88498244535465354 ) ) ;
#15031 = DIRECTION ( 'NONE',  ( 6.982962677686266711E-15, -0.000000000000000000, 1.000000000000000000 ) ) ;
#15032 = ORIENTED_EDGE ( 'NONE', *, *, #15121, .F. ) ;
#15033 = VECTOR ( 'NONE', #19948, 1000.000000000000000 ) ;
#15034 = ORIENTED_EDGE ( 'NONE', *, *, #15385, .T. ) ;
#15035 = CARTESIAN_POINT ( 'NONE',  ( -97.47038759843736955, -115.4903015188566826, 29.84619916992285837 ) ) ;
#15036 = EDGE_CURVE ( 'NONE', #19147, #4654, #806, .T. ) ;
#15037 = ADVANCED_FACE ( 'NONE', ( #4176 ), #10408, .F. ) ;
#15038 = ORIENTED_EDGE ( 'NONE', *, *, #9102, .T. ) ;
#15039 = CARTESIAN_POINT ( 'NONE',  ( -22.30005961346265408, -56.50329132715937419, 293.5832628385307999 ) ) ;
#15040 = PLANE ( 'NONE',  #17226 ) ;
#15041 = ORIENTED_EDGE ( 'NONE', *, *, #13238, .F. ) ;
#15042 = CARTESIAN_POINT ( 'NONE',  ( 91.89277925368698163, -118.5585056022113832, -7.620840104674680759 ) ) ;
#15043 = LINE ( 'NONE', #10524, #8319 ) ;
#15044 = EDGE_CURVE ( 'NONE', #16743, #14586, #10308, .T. ) ;
#15045 = CIRCLE ( 'NONE', #5918, 7.500000000000007105 ) ;
#15046 = CARTESIAN_POINT ( 'NONE',  ( 120.7779226595531128, 102.2982297021113141, 39.99999999999999289 ) ) ;
#15047 = FACE_OUTER_BOUND ( 'NONE', #17470, .T. ) ;
#15048 = DIRECTION ( 'NONE',  ( 0.7406645559057084549, -0.6718749999999998890, -9.546468602532142825E-17 ) ) ;
#15049 = DIRECTION ( 'NONE',  ( -0.8660254037844415942, 0.4999999999999950040, 0.000000000000000000 ) ) ;
#15050 = CYLINDRICAL_SURFACE ( 'NONE', #18604, 150.0000000000000284 ) ;
#15051 = CYLINDRICAL_SURFACE ( 'NONE', #10858, 9.999999999999994671 ) ;
#15052 = ORIENTED_EDGE ( 'NONE', *, *, #13698, .T. ) ;
#15053 = CARTESIAN_POINT ( 'NONE',  ( 7.948937137877743808, -60.22232964560488000, 293.5832628385307999 ) ) ;
#15054 = CARTESIAN_POINT ( 'NONE',  ( 159.9599531637113330, -36.50981547336952104, 39.99999999999999289 ) ) ;
#15055 = ORIENTED_EDGE ( 'NONE', *, *, #5060, .T. ) ;
#15056 = AXIS2_PLACEMENT_3D ( 'NONE', #3662, #5206, #13150 ) ;
#15057 = VERTEX_POINT ( 'NONE', #19625 ) ;
#15058 = EDGE_LOOP ( 'NONE', ( #5144, #14950, #1820 ) ) ;
#15059 = LINE ( 'NONE', #7195, #2491 ) ;
#15060 = ORIENTED_EDGE ( 'NONE', *, *, #10367, .F. ) ;
#15061 = CARTESIAN_POINT ( 'NONE',  ( 133.6865796038707117, -79.84358686291109564, 2.536759214717485111 ) ) ;
#15062 = CARTESIAN_POINT ( 'NONE',  ( -32.50000000000000000, 0.000000000000000000, 49.99999999999999289 ) ) ;
#15063 = CARTESIAN_POINT ( 'NONE',  ( -73.25972925305609351, 27.53920554013712874, 111.4180192758973931 ) ) ;
#15064 = CARTESIAN_POINT ( 'NONE',  ( -105.2664779077412192, -122.4188771607292949, 39.76387409687995245 ) ) ;
#15065 = CARTESIAN_POINT ( 'NONE',  ( 0.000000000000000000, 0.000000000000000000, 248.9926560891072143 ) ) ;
#15066 = VERTEX_POINT ( 'NONE', #6953 ) ;
#15067 = DIRECTION ( 'NONE',  ( -0.000000000000000000, -0.000000000000000000, -1.000000000000000000 ) ) ;
#15068 = CARTESIAN_POINT ( 'NONE',  ( -132.9648440817100266, -83.65857578542973272, 1.155905617014955755 ) ) ;
#15069 = CARTESIAN_POINT ( 'NONE',  ( 132.7722305162506302, -69.92010858955958952, 5.898643563562469438 ) ) ;
#15070 = DIRECTION ( 'NONE',  ( -0.000000000000000000, -0.000000000000000000, -1.000000000000000000 ) ) ;
#15071 = LINE ( 'NONE', #8731, #236 ) ;
#15072 = CARTESIAN_POINT ( 'NONE',  ( -134.7747342791601000, -65.84665809079258736, 34.80178653497117125 ) ) ;
#15073 = ORIENTED_EDGE ( 'NONE', *, *, #4220, .F. ) ;
#15074 =( REPRESENTATION_RELATIONSHIP ('NONE','NONE', #17382, #16185 ) REPRESENTATION_RELATIONSHIP_WITH_TRANSFORMATION ( #626 )SHAPE_REPRESENTATION_RELATIONSHIP( ) );
#15075 = ORIENTED_EDGE ( 'NONE', *, *, #14600, .F. ) ;
#15076 = ORIENTED_EDGE ( 'NONE', *, *, #8528, .F. ) ;
#15077 = ORIENTED_EDGE ( 'NONE', *, *, #16524, .T. ) ;
#15078 = ORIENTED_EDGE ( 'NONE', *, *, #17799, .F. ) ;
#15079 = EDGE_CURVE ( 'NONE', #6085, #17491, #5697, .T. ) ;
#15080 = CARTESIAN_POINT ( 'NONE',  ( -47.56244194535165803, -37.78198917157335046, 283.5832628385307999 ) ) ;
#15081 = CARTESIAN_POINT ( 'NONE',  ( 0.000000000000000000, 164.0736214083062805, 49.99999999999999289 ) ) ;
#15082 = ORIENTED_EDGE ( 'NONE', *, *, #5611, .F. ) ;
#15083 = AXIS2_PLACEMENT_3D ( 'NONE', #7619, #9050, #15297 ) ;
#15084 = LINE ( 'NONE', #8025, #6088 ) ;
#15085 = CARTESIAN_POINT ( 'NONE',  ( -109.9999999999983515, 285.0000000000000568, 85.00000000000001421 ) ) ;
#15086 = VERTEX_POINT ( 'NONE', #10023 ) ;
#15087 = FACE_OUTER_BOUND ( 'NONE', #13779, .T. ) ;
#15088 = DIRECTION ( 'NONE',  ( -0.7660444431189862291, -0.6427876096865298150, 4.304393070272780959E-15 ) ) ;
#15089 = CARTESIAN_POINT ( 'NONE',  ( -21.36933070621726571, 54.67896814532662830, 132.4711112102474146 ) ) ;
#15090 = CARTESIAN_POINT ( 'NONE',  ( 128.2779226595531270, 102.2982297021113141, 60.00000000000000000 ) ) ;
#15091 = ADVANCED_FACE ( 'NONE', ( #8783 ), #15022, .F. ) ;
#15092 = EDGE_CURVE ( 'NONE', #7122, #4330, #10214, .T. ) ;
#15093 = CARTESIAN_POINT ( 'NONE',  ( 133.0662791979978863, -83.15705346520361729, 38.69754810580496951 ) ) ;
#15094 = FACE_OUTER_BOUND ( 'NONE', #2891, .T. ) ;
#15095 = VERTEX_POINT ( 'NONE', #8487 ) ;
#15096 = ADVANCED_FACE ( 'NONE', ( #14723 ), #13174, .F. ) ;
#15097 = DIRECTION ( 'NONE',  ( 6.982962677686266711E-15, -0.000000000000000000, 1.000000000000000000 ) ) ;
#15098 = AXIS2_PLACEMENT_3D ( 'NONE', #4649, #46, #7910 ) ;
#15099 = VECTOR ( 'NONE', #7981, 1000.000000000000227 ) ;
#15100 = ORIENTED_EDGE ( 'NONE', *, *, #11279, .F. ) ;
#15101 = ORIENTED_EDGE ( 'NONE', *, *, #17750, .F. ) ;
#15102 = CARTESIAN_POINT ( 'NONE',  ( 0.000000000000000000, 0.000000000000000000, 293.5832628385307999 ) ) ;
#15103 = ORIENTED_EDGE ( 'NONE', *, *, #12825, .F. ) ;
#15104 = ORIENTED_EDGE ( 'NONE', *, *, #4911, .F. ) ;
#15105 = CIRCLE ( 'NONE', #4332, 112.8770930172170210 ) ;
#15106 = EDGE_CURVE ( 'NONE', #870, #14697, #2450, .T. ) ;
#15107 = DIRECTION ( 'NONE',  ( 1.000000000000000000, 0.000000000000000000, 0.000000000000000000 ) ) ;
#15108 = CYLINDRICAL_SURFACE ( 'NONE', #11234, 10.00000000000000000 ) ;
#15109 = FACE_OUTER_BOUND ( 'NONE', #17682, .T. ) ;
#15110 = LINE ( 'NONE', #1091, #823 ) ;
#15111 = CARTESIAN_POINT ( 'NONE',  ( 1.396592535537252080E-14, 0.000000000000000000, 49.99999999999998579 ) ) ;
#15112 = ORIENTED_EDGE ( 'NONE', *, *, #1472, .T. ) ;
#15113 = CARTESIAN_POINT ( 'NONE',  ( -128.2293354902420504, -77.84035270136639895, 48.15785137238516711 ) ) ;
#15115 = CIRCLE ( 'NONE', #1399, 9.999999999999994671 ) ;
#15114 = DIRECTION ( 'NONE',  ( 0.000000000000000000, 0.000000000000000000, -1.000000000000000000 ) ) ;
#15116 = VECTOR ( 'NONE', #2797, 1000.000000000000114 ) ;
#15117 = DIRECTION ( 'NONE',  ( 0.03505990758545895342, 0.9993852124581886764, 0.000000000000000000 ) ) ;
#15118 = VERTEX_POINT ( 'NONE', #10125 ) ;
#15119 = ADVANCED_FACE ( 'NONE', ( #8682 ), #18195, .F. ) ;
#15120 = LINE ( 'NONE', #1103, #13295 ) ;
#15121 = EDGE_CURVE ( 'NONE', #1501, #1401, #18123, .T. ) ;
#15122 = VECTOR ( 'NONE', #6425, 1000.000000000000000 ) ;
#15123 = LINE ( 'NONE', #2960, #4250 ) ;
#15124 = FACE_OUTER_BOUND ( 'NONE', #5681, .T. ) ;
#15125 = VERTEX_POINT ( 'NONE', #6131 ) ;
#15126 = ADVANCED_FACE ( 'NONE', ( #13575 ), #7345, .F. ) ;
#15127 = CYLINDRICAL_SURFACE ( 'NONE', #14954, 7.500000000000020428 ) ;
#15128 = DIRECTION ( 'NONE',  ( -0.000000000000000000, -1.000000000000000000, -0.000000000000000000 ) ) ;
#15129 = EDGE_LOOP ( 'NONE', ( #3672, #20015 ) ) ;
#15130 = ORIENTED_EDGE ( 'NONE', *, *, #19993, .T. ) ;
#15131 = LINE ( 'NONE', #12364, #7139 ) ;
#15132 = AXIS2_PLACEMENT_3D ( 'NONE', #3068, #9302, #6139 ) ;
#15133 = ORIENTED_EDGE ( 'NONE', *, *, #10382, .T. ) ;
#15134 = CARTESIAN_POINT ( 'NONE',  ( -55.16472960512350454, 30.25670013172272377, 132.4711112102474146 ) ) ;
#15135 = EDGE_CURVE ( 'NONE', #12020, #9612, #5819, .T. ) ;
#15136 = LINE ( 'NONE', #12159, #16459 ) ;
#15137 = EDGE_LOOP ( 'NONE', ( #11947, #2213 ) ) ;
#15138 = CIRCLE ( 'NONE', #18423, 77.50000000000000000 ) ;
#15139 = FACE_OUTER_BOUND ( 'NONE', #14542, .T. ) ;
#15140 = CARTESIAN_POINT ( 'NONE',  ( -110.0000000000000142, 265.0000000000000000, -82.50000000000001421 ) ) ;
#15141 = CARTESIAN_POINT ( 'NONE',  ( -136.4994460260982407, -31.11111111111750915, -10.83150941965273262 ) ) ;
#15142 = CARTESIAN_POINT ( 'NONE',  ( 85.53020504959901871, -140.9188050298377846, 49.99999999999999289 ) ) ;
#15143 = DIRECTION ( 'NONE',  ( -6.982962677686266711E-15, 0.000000000000000000, -1.000000000000000000 ) ) ;
#15144 = DIRECTION ( 'NONE',  ( 1.000000000000000000, 0.000000000000000000, -6.976128451377903642E-15 ) ) ;
#15145 = ADVANCED_FACE ( 'NONE', ( #1202 ), #9295, .F. ) ;
#15146 = LINE ( 'NONE', #2781, #15909 ) ;
#15147 = DIRECTION ( 'NONE',  ( 0.000000000000000000, 0.000000000000000000, -1.000000000000000000 ) ) ;
#15148 = DIRECTION ( 'NONE',  ( 1.000000000000000000, 0.000000000000000000, 0.000000000000000000 ) ) ;
#15149 = EDGE_CURVE ( 'NONE', #17276, #17652, #19117, .T. ) ;
#15150 = ORIENTED_EDGE ( 'NONE', *, *, #17778, .F. ) ;
#15151 = CARTESIAN_POINT ( 'NONE',  ( 181.0783081749256951, -199.9999999999999716, 40.00000000000000000 ) ) ;
#15152 = LINE ( 'NONE', #4208, #2710 ) ;
#15153 = ORIENTED_EDGE ( 'NONE', *, *, #555, .T. ) ;
#15154 = VECTOR ( 'NONE', #6687, 1000.000000000000227 ) ;
#15155 = EDGE_CURVE ( 'NONE', #18587, #16844, #16496, .T. ) ;
#15156 = ORIENTED_EDGE ( 'NONE', *, *, #8016, .F. ) ;
#15157 = AXIS2_PLACEMENT_3D ( 'NONE', #252, #12420, #17455 ) ;
#15158 = ADVANCED_FACE ( 'NONE', ( #2958 ), #3062, .T. ) ;
#15159 = ORIENTED_EDGE ( 'NONE', *, *, #4093, .F. ) ;
#15160 = DIRECTION ( 'NONE',  ( 0.2225209339563044841, 0.9749279121818258398, 0.000000000000000000 ) ) ;
#15161 = ORIENTED_EDGE ( 'NONE', *, *, #763, .T. ) ;
#15162 = CARTESIAN_POINT ( 'NONE',  ( 132.1979689506645173, -87.16940599486623853, 0.3707483414095501528 ) ) ;
#15163 = DIRECTION ( 'NONE',  ( -0.6692498792541753394, -0.7430374143461900838, 0.000000000000000000 ) ) ;
#15164 = CARTESIAN_POINT ( 'NONE',  ( 79.75827554147308263, 9.767571684737763671E-15, 269.6944534026102360 ) ) ;
#15165 = DIRECTION ( 'NONE',  ( 0.000000000000000000, 0.000000000000000000, -1.000000000000000000 ) ) ;
#15166 = CIRCLE ( 'NONE', #4394, 150.0000000000000284 ) ;
#15167 = CARTESIAN_POINT ( 'NONE',  ( 32.64570716507540737, -53.78543575132139409, 248.9926560891072143 ) ) ;
#15168 = VERTEX_POINT ( 'NONE', #18301 ) ;
#15169 = CYLINDRICAL_SURFACE ( 'NONE', #19920, 7.500000000000003553 ) ;
#15170 = CARTESIAN_POINT ( 'NONE',  ( -134.5985778548204905, -73.87143572891798726, 7.065257048864122424 ) ) ;
#15171 = CARTESIAN_POINT ( 'NONE',  ( 132.2954651231882792, -86.73864221000000896, 0.4534272278281766266 ) ) ;
#15172 = DIRECTION ( 'NONE',  ( 0.000000000000000000, 0.000000000000000000, -1.000000000000000000 ) ) ;
#15173 = CARTESIAN_POINT ( 'NONE',  ( -42.50000000000000000, 5.204748896376250896E-15, -120.0000000000000142 ) ) ;
#15174 = CARTESIAN_POINT ( 'NONE',  ( -134.6956030146838259, -73.12307453599522944, 31.50188018822290559 ) ) ;
#15175 = ORIENTED_EDGE ( 'NONE', *, *, #5861, .T. ) ;
#15176 = CARTESIAN_POINT ( 'NONE',  ( -9.176097008934114285, -25.21111933077039069, 14.88498244535551507 ) ) ;
#15177 = EDGE_CURVE ( 'NONE', #15284, #7659, #20033, .T. ) ;
#15178 = EDGE_LOOP ( 'NONE', ( #5883, #16430, #18541, #5240 ) ) ;
#15179 = ORIENTED_EDGE ( 'NONE', *, *, #2364, .F. ) ;
#15180 = VECTOR ( 'NONE', #18150, 1000.000000000000114 ) ;
#15181 = VERTEX_POINT ( 'NONE', #1521 ) ;
#15182 = VERTEX_POINT ( 'NONE', #10816 ) ;
#15183 = CARTESIAN_POINT ( 'NONE',  ( -110.0000000000000142, 275.0000000000000000, 39.99999999999997868 ) ) ;
#15184 = CARTESIAN_POINT ( 'NONE',  ( 7.950000000000000178, 5.196152422706624030, -9.000000000000001776 ) ) ;
#15185 = CARTESIAN_POINT ( 'NONE',  ( -28.06584155524099700, 53.86996498385662591, 293.5832628385307999 ) ) ;
#15186 = ORIENTED_EDGE ( 'NONE', *, *, #10096, .F. ) ;
#15188 = CARTESIAN_POINT ( 'NONE',  ( -32.16802499836779106, -54.07248341783242296, 248.9926560891072143 ) ) ;
#15187 = AXIS2_PLACEMENT_3D ( 'NONE', #3678, #13264, #11549 ) ;
#15189 = DIRECTION ( 'NONE',  ( 0.000000000000000000, 0.000000000000000000, 1.000000000000000000 ) ) ;
#15190 = EDGE_LOOP ( 'NONE', ( #7316, #9041, #7482, #11589 ) ) ;
#15191 = CYLINDRICAL_SURFACE ( 'NONE', #1595, 60.74260934110282051 ) ;
#15192 = CARTESIAN_POINT ( 'NONE',  ( 0.000000000000000000, 0.000000000000000000, 283.5832628385307999 ) ) ;
#15193 = CARTESIAN_POINT ( 'NONE',  ( -3.221721112346616067, 26.95290724009910832, 14.88498244535547244 ) ) ;
#15194 = CARTESIAN_POINT ( 'NONE',  ( -189.9999999999988916, 275.0000000000000000, -2.499999999999734879 ) ) ;
#15195 = CARTESIAN_POINT ( 'NONE',  ( -58.69016442926522359, 0.8220851292433277724, 248.9926560891072143 ) ) ;
#15196 = AXIS2_PLACEMENT_3D ( 'NONE', #5158, #12604, #18867 ) ;
#15197 = ORIENTED_EDGE ( 'NONE', *, *, #7504, .F. ) ;
#15198 = EDGE_CURVE ( 'NONE', #19395, #10591, #1421, .T. ) ;
#15199 = CARTESIAN_POINT ( 'NONE',  ( -176.1792632384392050, -186.5724904703759535, 30.00000000000000000 ) ) ;
#15200 = VERTEX_POINT ( 'NONE', #10503 ) ;
#15201 = ORIENTED_EDGE ( 'NONE', *, *, #14749, .T. ) ;
#15202 = CARTESIAN_POINT ( 'NONE',  ( 38.41834839689379777, -68.18670162478818497, 248.9926560891072143 ) ) ;
#15203 = ORIENTED_EDGE ( 'NONE', *, *, #9530, .T. ) ;
#15204 = ORIENTED_EDGE ( 'NONE', *, *, #6618, .T. ) ;
#15205 = CARTESIAN_POINT ( 'NONE',  ( 28.06281046684275182, -73.06915264522010034, 248.9926560891072143 ) ) ;
#15206 = EDGE_CURVE ( 'NONE', #18899, #16800, #20090, .T. ) ;
#15207 = FILL_AREA_STYLE_COLOUR ( '', #12529 ) ;
#15208 = CARTESIAN_POINT ( 'NONE',  ( 0.000000000000000000, -7.794228634059948035, -4.499999999999999112 ) ) ;
#15209 = ORIENTED_EDGE ( 'NONE', *, *, #4273, .F. ) ;
#15210 = CARTESIAN_POINT ( 'NONE',  ( 0.1469846612282481035, 6.696526368584462041, -6.401276095386996268 ) ) ;
#15211 = LINE ( 'NONE', #5513, #18807 ) ;
#15212 = CIRCLE ( 'NONE', #542, 60.74260934110282051 ) ;
#15213 = ORIENTED_EDGE ( 'NONE', *, *, #4883, .F. ) ;
#15214 = FACE_BOUND ( 'NONE', #15395, .T. ) ;
#15215 = DIRECTION ( 'NONE',  ( -0.000000000000000000, -0.000000000000000000, 1.000000000000000000 ) ) ;
#15216 = CIRCLE ( 'NONE', #16177, 3.224098631618460775 ) ;
#15217 = LINE ( 'NONE', #12248, #12567 ) ;
#15218 = VERTEX_POINT ( 'NONE', #4590 ) ;
#15219 = LINE ( 'NONE', #10411, #880 ) ;
#15220 = CARTESIAN_POINT ( 'NONE',  ( -134.6804726163186388, -73.23883837743913716, 31.68330670238580282 ) ) ;
#15221 = CARTESIAN_POINT ( 'NONE',  ( -90.70229574719763832, 106.6474785866378312, 34.20743887950242623 ) ) ;
#15222 = VERTEX_POINT ( 'NONE', #8976 ) ;
#15223 = EDGE_CURVE ( 'NONE', #18597, #12045, #15217, .T. ) ;
#15224 = FACE_BOUND ( 'NONE', #4450, .T. ) ;
#15225 = CARTESIAN_POINT ( 'NONE',  ( -60.72073886220397299, 1.629865514042312613, 283.5832628385307999 ) ) ;
#15226 = ORIENTED_EDGE ( 'NONE', *, *, #9980, .T. ) ;
#15227 = AXIS2_PLACEMENT_3D ( 'NONE', #18001, #4070, #5612 ) ;
#15228 = ORIENTED_EDGE ( 'NONE', *, *, #17094, .F. ) ;
#15229 = CARTESIAN_POINT ( 'NONE',  ( -98.53720805795876458, -132.5762351826747931, 34.43852096856275580 ) ) ;
#15230 = AXIS2_PLACEMENT_3D ( 'NONE', #9382, #15727, #12544 ) ;
#15231 = EDGE_LOOP ( 'NONE', ( #12656, #3456, #18481, #18567 ) ) ;
#15232 = FACE_OUTER_BOUND ( 'NONE', #1665, .T. ) ;
#15233 = AXIS2_PLACEMENT_3D ( 'NONE', #16839, #4567, #2731 ) ;
#15234 = EDGE_CURVE ( 'NONE', #19683, #9722, #13990, .T. ) ;
#15235 = DIRECTION ( 'NONE',  ( 0.000000000000000000, 1.000000000000000000, 0.000000000000000000 ) ) ;
#15236 = VERTEX_POINT ( 'NONE', #12453 ) ;
#15237 = CARTESIAN_POINT ( 'NONE',  ( 95.87485967515245022, -116.0949201519035370, 9.456033085400639138 ) ) ;
#15238 = CARTESIAN_POINT ( 'NONE',  ( -9.176097008934114285, -25.21111933077039069, 14.88498244535551507 ) ) ;
#15239 = EDGE_CURVE ( 'NONE', #17104, #18698, #13889, .T. ) ;
#15240 = AXIS2_PLACEMENT_3D ( 'NONE', #15192, #16835, #17148 ) ;
#15241 = CARTESIAN_POINT ( 'NONE',  ( -136.1355222778962570, -24.69918106743299901, -20.28146826871829589 ) ) ;
#15242 = CYLINDRICAL_SURFACE ( 'NONE', #10817, 60.74260934110282051 ) ;
#15243 = FACE_OUTER_BOUND ( 'NONE', #4694, .T. ) ;
#15244 = CYLINDRICAL_SURFACE ( 'NONE', #16895, 79.75827554147308263 ) ;
#15245 = CARTESIAN_POINT ( 'NONE',  ( -25.74015858913164578, 7.810105800529631992, 14.88498244535563231 ) ) ;
#15246 = DIRECTION ( 'NONE',  ( -0.000000000000000000, -0.000000000000000000, 1.000000000000000000 ) ) ;
#15247 = ORIENTED_EDGE ( 'NONE', *, *, #8468, .T. ) ;
#15248 = VECTOR ( 'NONE', #18008, 1000.000000000000000 ) ;
#15249 = EDGE_CURVE ( 'NONE', #20227, #12671, #17182, .T. ) ;
#15250 = FACE_OUTER_BOUND ( 'NONE', #14486, .T. ) ;
#15251 = CARTESIAN_POINT ( 'NONE',  ( -19.30071112029641967, 55.43188410062188609, 111.4180192758973931 ) ) ;
#15252 = ORIENTED_EDGE ( 'NONE', *, *, #14869, .T. ) ;
#15253 = ORIENTED_EDGE ( 'NONE', *, *, #5772, .F. ) ;
#15254 = ORIENTED_EDGE ( 'NONE', *, *, #10595, .T. ) ;
#15255 = DIRECTION ( 'NONE',  ( 0.000000000000000000, 0.000000000000000000, -1.000000000000000000 ) ) ;
#15256 = ORIENTED_EDGE ( 'NONE', *, *, #17111, .F. ) ;
#15257 = EDGE_CURVE ( 'NONE', #19127, #11748, #13683, .T. ) ;
#15258 = DIRECTION ( 'NONE',  ( 0.000000000000000000, 0.000000000000000000, 1.000000000000000000 ) ) ;
#15259 = CARTESIAN_POINT ( 'NONE',  ( 134.5748517645101572, -74.05062141148569310, 6.795614893174752424 ) ) ;
#15260 = DIRECTION ( 'NONE',  ( -0.9511061040868794558, -0.3088643371590157338, 0.000000000000000000 ) ) ;
#15261 = CIRCLE ( 'NONE', #15612, 7.500000000000020428 ) ;
#15262 = EDGE_CURVE ( 'NONE', #13232, #5703, #6385, .T. ) ;
#15263 =( BOUNDED_SURFACE ( )  B_SPLINE_SURFACE ( 3, 2, ( 
 ( #13933, #20178, #4847 ),
 ( #18761, #11069, #17224 ),
 ( #3205, #13100, #9839 ),
 ( #6688, #6880, #12908 ),
 ( #13290, #19458, #10047 ),
 ( #19358, #11475, #14748 ),
 ( #13006, #14648, #19161 ),
 ( #2183, #11576, #437 ),
 ( #19268, #17828, #16092 ),
 ( #8306, #17729, #8408 ),
 ( #3706, #8605, #17636 ),
 ( #3800, #6974, #13193 ),
 ( #2081, #14840, #19548 ),
 ( #16392, #729, #11762 ),
 ( #18024, #9945, #10140 ),
 ( #3993, #5441, #5249 ),
 ( #6784, #16195, #825 ),
 ( #3901, #637, #10234 ),
 ( #11668, #5346, #16296 ),
 ( #8508, #2280, #14553 ),
 ( #5155, #17929, #11380 ),
 ( #5541, #2371, #7076 ),
 ( #16490, #8206, #14452 ),
 ( #3607, #540, #13394 ),
 ( #16685, #5839, #14935 ),
 ( #13492, #12058, #10327 ),
 ( #2567, #5741, #2672 ),
 ( #11953, #2873, #11856 ) ),
 .UNSPECIFIED., .F., .F., .F. ) 
 B_SPLINE_SURFACE_WITH_KNOTS ( ( 4, 2, 2, 2, 2, 2, 2, 2, 2, 2, 2, 2, 2, 4 ),
 ( 3, 3 ),
 ( 0.01172725363905311943, 0.01619455768277540397, 0.01731138369370597424, 0.01842820970463654451, 0.02066186172649768504, 0.02289551374835882558, 0.02401233975928939585, 0.02512916577021996958, 0.02959646981394225412, 0.03406377385766454213, 0.03629742587952568267, 0.03853107790138682320, 0.04299838194510910427, 0.04746568598883138534 ),
 ( 0.000000000000000000, 1.000000000000000000 ),
 .UNSPECIFIED. ) 
 GEOMETRIC_REPRESENTATION_ITEM ( )  RATIONAL_B_SPLINE_SURFACE ( (
 ( 1.000000000000000000, 0.4759858191164941243, 1.000000000000000000),
 ( 1.000000000000000000, 0.4759956267211572500, 1.000000000000000000),
 ( 1.000000000000000000, 0.4778541562213696192, 1.000000000000000000),
 ( 1.000000000000000000, 0.4823973722701895839, 1.000000000000000000),
 ( 1.000000000000000000, 0.4834178931535008661, 1.000000000000000000),
 ( 1.000000000000000000, 0.4856852555523819004, 1.000000000000000000),
 ( 1.000000000000000000, 0.4869309269816905483, 1.000000000000000000),
 ( 1.000000000000000000, 0.4909487690765744761, 1.000000000000000000),
 ( 1.000000000000000000, 0.4940161083580011936, 1.000000000000000000),
 ( 1.000000000000000000, 0.5008835903390457256, 1.000000000000000000),
 ( 1.000000000000000000, 0.5046839780478528104, 1.000000000000000000),
 ( 1.000000000000000000, 0.5109205925582557262, 1.000000000000000000),
 ( 1.000000000000000000, 0.5130943221002354226, 1.000000000000000000),
 ( 1.000000000000000000, 0.5175691686948765691, 1.000000000000000000),
 ( 1.000000000000000000, 0.5198746620754810532, 1.000000000000000000),
 ( 1.000000000000000000, 0.5317265360209684211, 1.000000000000000000),
 ( 1.000000000000000000, 0.5422380167215470337, 1.000000000000000000),
 ( 1.000000000000000000, 0.5650731438342535551, 1.000000000000000000),
 ( 1.000000000000000000, 0.5770759225151705918, 1.000000000000000000),
 ( 1.000000000000000000, 0.5957780208533434152, 1.000000000000000000),
 ( 1.000000000000000000, 0.6021295156452242114, 1.000000000000000000),
 ( 1.000000000000000000, 0.6150481322456406996, 1.000000000000000000),
 ( 1.000000000000000000, 0.6215784740531448138, 1.000000000000000000),
 ( 1.000000000000000000, 0.6411710492557047836, 1.000000000000000000),
 ( 1.000000000000000000, 0.6543107498251993226, 1.000000000000000000),
 ( 1.000000000000000000, 0.6806663510245557491, 1.000000000000000000),
 ( 1.000000000000000000, 0.6938871677785066749, 1.000000000000000000),
 ( 1.000000000000000000, 0.7071067811865475727, 1.000000000000000000) ) ) 
 REPRESENTATION_ITEM ( '' )  SURFACE ( )  );
#15264 = AXIS2_PLACEMENT_3D ( 'NONE', #17285, #15540, #12558 ) ;
#15265 = CARTESIAN_POINT ( 'NONE',  ( 97.50000000000002842, -195.8578643762690206, 4.142135623730952787 ) ) ;
#15266 = CIRCLE ( 'NONE', #5476, 32.50000000000000000 ) ;
#15267 = CARTESIAN_POINT ( 'NONE',  ( -100.7812499999999716, -111.0996833858562951, 50.00000000000000000 ) ) ;
#15268 = CARTESIAN_POINT ( 'NONE',  ( -51.24071425735602503, 32.61983739937743820, 293.5832628385307999 ) ) ;
#15269 = ORIENTED_EDGE ( 'NONE', *, *, #2640, .F. ) ;
#15270 = CARTESIAN_POINT ( 'NONE',  ( 0.000000000000000000, 0.000000000000000000, 283.5832628385307999 ) ) ;
#15271 = CARTESIAN_POINT ( 'NONE',  ( -131.8415137303880726, -71.65490762083834397, 3.257559711240717526 ) ) ;
#15272 = CARTESIAN_POINT ( 'NONE',  ( 131.4291603288649242, -72.40192386451009554, 2.550978253286948938 ) ) ;
#15273 = CARTESIAN_POINT ( 'NONE',  ( 0.000000000000000000, 0.000000000000000000, 49.99999999999999289 ) ) ;
#15274 = LINE ( 'NONE', #15173, #6128 ) ;
#15275 = CARTESIAN_POINT ( 'NONE',  ( 107.5000000000000284, -199.9999999999999716, 40.00000000000000000 ) ) ;
#15276 = ORIENTED_EDGE ( 'NONE', *, *, #1081, .T. ) ;
#15277 = EDGE_CURVE ( 'NONE', #16849, #9808, #2854, .T. ) ;
#15278 = CARTESIAN_POINT ( 'NONE',  ( 0.000000000000000000, 0.000000000000000000, 0.000000000000000000 ) ) ;
#15279 = CIRCLE ( 'NONE', #4181, 62.91752772691707207 ) ;
#15280 = CIRCLE ( 'NONE', #12322, 62.91752772691707207 ) ;
#15281 = VERTEX_POINT ( 'NONE', #4484 ) ;
#15282 = EDGE_LOOP ( 'NONE', ( #17079, #17053, #10697, #25 ) ) ;
#15283 = ADVANCED_BREP_SHAPE_REPRESENTATION ( '', ( #1084, #18639 ), #4580 ) ;
#15284 = VERTEX_POINT ( 'NONE', #20131 ) ;
#15285 = EDGE_CURVE ( 'NONE', #4813, #10391, #1931, .T. ) ;
#15286 = DIRECTION ( 'NONE',  ( 0.000000000000000000, 0.000000000000000000, 1.000000000000000000 ) ) ;
#15287 = LINE ( 'NONE', #9565, #15830 ) ;
#15288 = DIRECTION ( 'NONE',  ( -0.000000000000000000, -0.000000000000000000, 1.000000000000000000 ) ) ;
#15289 = ORIENTED_EDGE ( 'NONE', *, *, #13842, .F. ) ;
#15290 = PLANE ( 'NONE',  #10981 ) ;
#15291 = DIRECTION ( 'NONE',  ( -0.000000000000000000, -0.000000000000000000, 1.000000000000000000 ) ) ;
#15292 = CIRCLE ( 'NONE', #12355, 10.00000000000000178 ) ;
#15293 = ADVANCED_FACE ( 'NONE', ( #12557 ), #14096, .T. ) ;
#15294 = ORIENTED_EDGE ( 'NONE', *, *, #19486, .F. ) ;
#15295 = DIRECTION ( 'NONE',  ( -1.000000000000000000, 0.000000000000000000, 0.000000000000000000 ) ) ;
#15296 = AXIS2_PLACEMENT_3D ( 'NONE', #2267, #19635, #5527 ) ;
#15297 = DIRECTION ( 'NONE',  ( -0.9848077530122073542, -0.1736481776669340227, 0.000000000000000000 ) ) ;
#15298 = CARTESIAN_POINT ( 'NONE',  ( -134.1103769904814840, -77.28650662340044164, 3.884190938604082266 ) ) ;
#15299 = PLANE ( 'NONE',  #18322 ) ;
#15300 = LINE ( 'NONE', #1292, #4849 ) ;
#15301 = CARTESIAN_POINT ( 'NONE',  ( -49.67518383744793908, 60.47951622432801599, 110.7293897666001214 ) ) ;
#15302 = VERTEX_POINT ( 'NONE', #9796 ) ;
#15303 = VERTEX_POINT ( 'NONE', #9500 ) ;
#15304 = DIRECTION ( 'NONE',  ( 0.000000000000000000, 0.000000000000000000, -1.000000000000000000 ) ) ;
#15305 = CIRCLE ( 'NONE', #18244, 9.000000000000000000 ) ;
#15306 = ORIENTED_EDGE ( 'NONE', *, *, #2102, .F. ) ;
#15307 = AXIS2_PLACEMENT_3D ( 'NONE', #2131, #8158, #10098 ) ;
#15308 = VERTEX_POINT ( 'NONE', #17488 ) ;
#15309 = DIRECTION ( 'NONE',  ( 1.000000000000000000, 0.000000000000000000, 0.000000000000000000 ) ) ;
#15310 = CIRCLE ( 'NONE', #8129, 9.000000000000000000 ) ;
#15311 = ORIENTED_EDGE ( 'NONE', *, *, #685, .F. ) ;
#15312 = ORIENTED_EDGE ( 'NONE', *, *, #7039, .F. ) ;
#15313 = CARTESIAN_POINT ( 'NONE',  ( -110.0000000000000142, 275.0000000000000000, 5.000000000000000888 ) ) ;
#15314 = FACE_OUTER_BOUND ( 'NONE', #4619, .T. ) ;
#15315 = ORIENTED_EDGE ( 'NONE', *, *, #3870, .T. ) ;
#15316 = DIRECTION ( 'NONE',  ( -0.000000000000000000, -0.000000000000000000, 1.000000000000000000 ) ) ;
#15317 = DIRECTION ( 'NONE',  ( 1.000000000000000000, 0.000000000000000000, 0.000000000000000000 ) ) ;
#15318 = VECTOR ( 'NONE', #9953, 1000.000000000000000 ) ;
#15319 = ORIENTED_EDGE ( 'NONE', *, *, #6884, .T. ) ;
#15320 = DIRECTION ( 'NONE',  ( -1.000000000000000000, 0.000000000000000000, -0.000000000000000000 ) ) ;
#15321 = DIRECTION ( 'NONE',  ( 6.982962677686266711E-15, -0.000000000000000000, 1.000000000000000000 ) ) ;
#15322 = VECTOR ( 'NONE', #2076, 1000.000000000000114 ) ;
#15323 = CIRCLE ( 'NONE', #4211, 62.91752772691707207 ) ;
#15324 = CARTESIAN_POINT ( 'NONE',  ( 61.70726652483817531, 12.28122767885865407, 293.5832628385307999 ) ) ;
#15325 = DIRECTION ( 'NONE',  ( -0.9009688679024160374, -0.4338837391175646707, 0.000000000000000000 ) ) ;
#15326 = CARTESIAN_POINT ( 'NONE',  ( -150.0000000000000284, 0.000000000000000000, 49.99999999999999289 ) ) ;
#15327 = CARTESIAN_POINT ( 'NONE',  ( -95.40135526861702431, 102.4752410541829306, 36.83510734335156656 ) ) ;
#15328 = ORIENTED_EDGE ( 'NONE', *, *, #3182, .T. ) ;
#15329 = FACE_BOUND ( 'NONE', #17343, .T. ) ;
#15330 = CARTESIAN_POINT ( 'NONE',  ( 40.28046525994349736, 45.46865632508086463, 283.5832628385307999 ) ) ;
#15331 = EDGE_LOOP ( 'NONE', ( #16083, #5090, #19455, #3430 ) ) ;
#15332 = ORIENTED_EDGE ( 'NONE', *, *, #1752, .F. ) ;
#15333 = DIRECTION ( 'NONE',  ( 0.000000000000000000, 0.000000000000000000, -1.000000000000000000 ) ) ;
#15334 = ORIENTED_EDGE ( 'NONE', *, *, #18863, .F. ) ;
#15335 = AXIS2_PLACEMENT_3D ( 'NONE', #1088, #5708, #4064 ) ;
#15336 = CIRCLE ( 'NONE', #16002, 106.4288957539801004 ) ;
#15337 = CARTESIAN_POINT ( 'NONE',  ( 0.000000000000000000, 0.000000000000000000, 283.5832628385307999 ) ) ;
#15338 = FACE_OUTER_BOUND ( 'NONE', #4947, .T. ) ;
#15339 = ORIENTED_EDGE ( 'NONE', *, *, #14489, .F. ) ;
#15340 = CARTESIAN_POINT ( 'NONE',  ( 96.05830942202625522, -116.0381168402492023, 9.733529271712557218 ) ) ;
#15341 = DIRECTION ( 'NONE',  ( 0.000000000000000000, 0.000000000000000000, 1.000000000000000000 ) ) ;
#15342 = EDGE_CURVE ( 'NONE', #7173, #7971, #12958, .T. ) ;
#15343 = CARTESIAN_POINT ( 'NONE',  ( -141.3095340546368277, -18.69392313914324788, -14.89730798426476888 ) ) ;
#15344 = DIRECTION ( 'NONE',  ( 0.4693298356057564180, -0.8830229359480272766, 0.000000000000000000 ) ) ;
#15345 = FILL_AREA_STYLE ('',( #9420 ) ) ;
#15346 = DIRECTION ( 'NONE',  ( 0.6234898018587442525, -0.7818314824680211439, 0.000000000000000000 ) ) ;
#15347 = AXIS2_PLACEMENT_3D ( 'NONE', #1678, #9745, #17640 ) ;
#15348 = PLANE ( 'NONE',  #14606 ) ;
#15349 = DIRECTION ( 'NONE',  ( 0.000000000000000000, 0.000000000000000000, 1.000000000000000000 ) ) ;
#15350 = VECTOR ( 'NONE', #12811, 1000.000000000000227 ) ;
#15351 = CARTESIAN_POINT ( 'NONE',  ( 96.25554516486297985, -115.9717118653463785, 30.02399084163740284 ) ) ;
#15352 = ORIENTED_EDGE ( 'NONE', *, *, #1534, .F. ) ;
#15353 = ADVANCED_FACE ( 'NONE', ( #3360 ), #12863, .F. ) ;
#15354 = FACE_OUTER_BOUND ( 'NONE', #8622, .T. ) ;
#15355 = DIRECTION ( 'NONE',  ( 0.000000000000000000, 0.000000000000000000, 1.000000000000000000 ) ) ;
#15356 = ADVANCED_FACE ( 'NONE', ( #1825 ), #11024, .F. ) ;
#15357 = VERTEX_POINT ( 'NONE', #15945 ) ;
#15358 = ADVANCED_FACE ( 'NONE', ( #3461 ), #18923, .F. ) ;
#15359 = ORIENTED_EDGE ( 'NONE', *, *, #388, .F. ) ;
#15360 = CARTESIAN_POINT ( 'NONE',  ( -110.0000000000000426, 292.9500000000000455, -75.00000000000000000 ) ) ;
#15361 = EDGE_LOOP ( 'NONE', ( #6986, #10343, #6748, #16731 ) ) ;
#15362 = AXIS2_PLACEMENT_3D ( 'NONE', #10027, #16278, #5933 ) ;
#15363 = FACE_BOUND ( 'NONE', #16898, .T. ) ;
#15364 = ORIENTED_EDGE ( 'NONE', *, *, #3742, .F. ) ;
#15365 = VECTOR ( 'NONE', #10213, 1000.000000000000227 ) ;
#15366 = CARTESIAN_POINT ( 'NONE',  ( -51.51682027493045979, 28.15057869795642986, 110.9660488491356887 ) ) ;
#15367 = DIRECTION ( 'NONE',  ( 0.000000000000000000, 0.000000000000000000, 1.000000000000000000 ) ) ;
#15368 = LINE ( 'NONE', #12292, #18877 ) ;
#15369 = EDGE_CURVE ( 'NONE', #2720, #20112, #8057, .T. ) ;
#15370 = CARTESIAN_POINT ( 'NONE',  ( 101.6421356237309794, -200.0000000000000000, 4.186828437777334426E-15 ) ) ;
#15371 = LINE ( 'NONE', #5867, #6497 ) ;
#15372 = FACE_OUTER_BOUND ( 'NONE', #14137, .T. ) ;
#15373 = ORIENTED_EDGE ( 'NONE', *, *, #12348, .T. ) ;
#15374 = DIRECTION ( 'NONE',  ( 0.9396926207859063185, -0.3420201433256742640, -6.456589605409180904E-15 ) ) ;
#15375 = CARTESIAN_POINT ( 'NONE',  ( 48.72193424476451895, 39.80940113486035159, 248.9926560891072143 ) ) ;
#15376 = CARTESIAN_POINT ( 'NONE',  ( 130.0495322079418372, -74.74954793754227467, -6.424697538702346833 ) ) ;
#15377 = CARTESIAN_POINT ( 'NONE',  ( -163.5019688434124419, -20.99123081650240863, 39.99999999999999289 ) ) ;
#15378 = CYLINDRICAL_SURFACE ( 'NONE', #16063, 34.99999999999997868 ) ;
#15379 = CARTESIAN_POINT ( 'NONE',  ( -131.2164711380630990, -72.78471332658050130, 37.79149633612817638 ) ) ;
#15380 = ORIENTED_EDGE ( 'NONE', *, *, #6919, .T. ) ;
#15381 = VECTOR ( 'NONE', #10895, 1000.000000000000114 ) ;
#15382 = CARTESIAN_POINT ( 'NONE',  ( -41.48948842197086151, 47.29944656917798795, 293.5832628385307999 ) ) ;
#15383 = ADVANCED_FACE ( 'NONE', ( #6440 ), #14309, .F. ) ;
#15384 = AXIS2_PLACEMENT_3D ( 'NONE', #15273, #20082, #1262 ) ;
#15385 = EDGE_CURVE ( 'NONE', #18152, #6652, #1804, .T. ) ;
#15386 = ORIENTED_EDGE ( 'NONE', *, *, #20115, .T. ) ;
#15387 = ORIENTED_EDGE ( 'NONE', *, *, #11907, .T. ) ;
#15388 = CIRCLE ( 'NONE', #18678, 160.0000000000000284 ) ;
#15389 = EDGE_LOOP ( 'NONE', ( #19475, #17060, #792, #5582 ) ) ;
#15390 = CARTESIAN_POINT ( 'NONE',  ( -139.5534466488780936, -22.43207410479775277, 23.76218694605343984 ) ) ;
#15391 = VECTOR ( 'NONE', #18343, 1000.000000000000227 ) ;
#15392 = EDGE_CURVE ( 'NONE', #18157, #10298, #2443, .T. ) ;
#15393 = DIRECTION ( 'NONE',  ( -0.000000000000000000, -0.000000000000000000, 1.000000000000000000 ) ) ;
#15394 = DIRECTION ( 'NONE',  ( 0.000000000000000000, 0.4999999999999998335, -0.8660254037844387076 ) ) ;
#15395 = EDGE_LOOP ( 'NONE', ( #6017, #6280 ) ) ;
#15396 =( GEOMETRIC_REPRESENTATION_CONTEXT ( 3 ) GLOBAL_UNCERTAINTY_ASSIGNED_CONTEXT ( ( #13763 ) ) GLOBAL_UNIT_ASSIGNED_CONTEXT ( ( #3711, #16305, #19365 ) ) REPRESENTATION_CONTEXT ( 'NONE', 'WORKASPACE' ) );
#15397 = DIRECTION ( 'NONE',  ( 0.000000000000000000, 0.000000000000000000, 1.000000000000000000 ) ) ;
#15398 = CARTESIAN_POINT ( 'NONE',  ( 40.28046525994349736, 45.46865632508086463, 293.5832628385307999 ) ) ;
#15399 = ORIENTED_EDGE ( 'NONE', *, *, #15480, .T. ) ;
#15400 = CARTESIAN_POINT ( 'NONE',  ( -81.18278579426254282, 113.5842013066641130, -14.89122930995394256 ) ) ;
#15401 = DIRECTION ( 'NONE',  ( -0.3420201433256568890, -0.9396926207859126468, -0.000000000000000000 ) ) ;
#15402 = DIRECTION ( 'NONE',  ( -0.000000000000000000, -0.000000000000000000, 1.000000000000000000 ) ) ;
#15403 = CARTESIAN_POINT ( 'NONE',  ( 0.01885174614965864567, 0.8831628876357825453, 9.000000000000000000 ) ) ;
#15404 = DIRECTION ( 'NONE',  ( -0.6692498792541753394, -0.7430374143461900838, 0.000000000000000000 ) ) ;
#15405 = EDGE_CURVE ( 'NONE', #6447, #19359, #1628, .T. ) ;
#15406 = CARTESIAN_POINT ( 'NONE',  ( -62.90240729679781850, -1.379293853801974779, 248.9926560891072143 ) ) ;
#15407 = DIRECTION ( 'NONE',  ( -0.000000000000000000, -0.000000000000000000, 1.000000000000000000 ) ) ;
#15408 = EDGE_CURVE ( 'NONE', #15066, #18605, #12241, .T. ) ;
#15409 = ORIENTED_EDGE ( 'NONE', *, *, #19509, .T. ) ;
#15410 = ORIENTED_EDGE ( 'NONE', *, *, #2142, .T. ) ;
#15411 = CARTESIAN_POINT ( 'NONE',  ( 42.44352287704968063, 94.20918150411493741, 14.88498244535515624 ) ) ;
#15412 = EDGE_LOOP ( 'NONE', ( #10798, #20109, #16078, #1164 ) ) ;
#15413 = EDGE_CURVE ( 'NONE', #2014, #9259, #14540, .T. ) ;
#15414 = VERTEX_POINT ( 'NONE', #14506 ) ;
#15415 = CARTESIAN_POINT ( 'NONE',  ( -0.8220851292435327196, -58.69016442926522359, 112.7772637782949943 ) ) ;
#15416 = EDGE_CURVE ( 'NONE', #7173, #13146, #7032, .T. ) ;
#15417 = VECTOR ( 'NONE', #15916, 1000.000000000000000 ) ;
#15418 = ORIENTED_EDGE ( 'NONE', *, *, #8007, .T. ) ;
#15419 = DIRECTION ( 'NONE',  ( -0.9396926207859046531, -0.3420201433256790380, 0.000000000000000000 ) ) ;
#15420 = CARTESIAN_POINT ( 'NONE',  ( 28.06281046684275182, -73.06915264522012876, 132.4711112102474146 ) ) ;
#15421 = DIRECTION ( 'NONE',  ( -0.000000000000000000, -0.000000000000000000, 1.000000000000000000 ) ) ;
#15422 = DIRECTION ( 'NONE',  ( 1.000000000000000000, 0.000000000000000000, -6.977185866873308817E-15 ) ) ;
#15423 = ORIENTED_EDGE ( 'NONE', *, *, #11773, .F. ) ;
#15424 = DIRECTION ( 'NONE',  ( 0.03505990758545895342, 0.9993852124581886764, 0.000000000000000000 ) ) ;
#15425 = CARTESIAN_POINT ( 'NONE',  ( 73.82206860051530839, 25.99419088092216867, 132.4711112102474146 ) ) ;
#15426 = ORIENTED_EDGE ( 'NONE', *, *, #5405, .T. ) ;
#15427 = DIRECTION ( 'NONE',  ( -1.000000000000000000, 0.000000000000000000, 0.000000000000000000 ) ) ;
#15428 = LINE ( 'NONE', #9185, #1608 ) ;
#15429 = DIRECTION ( 'NONE',  ( 0.000000000000000000, 0.000000000000000000, -1.000000000000000000 ) ) ;
#15430 = CIRCLE ( 'NONE', #15098, 7.500000000000003553 ) ;
#15431 = AXIS2_PLACEMENT_3D ( 'NONE', #735, #6792, #16200 ) ;
#15432 = LINE ( 'NONE', #1422, #19522 ) ;
#15433 = CARTESIAN_POINT ( 'NONE',  ( -134.7188131032333445, -72.93593548660989256, 30.00000000000000000 ) ) ;
#15434 = CARTESIAN_POINT ( 'NONE',  ( -87.29829728531822752, 109.4572494691238518, 31.67964062618897003 ) ) ;
#15435 = ORIENTED_EDGE ( 'NONE', *, *, #10609, .F. ) ;
#15436 = DIRECTION ( 'NONE',  ( 0.000000000000000000, 0.000000000000000000, 1.000000000000000000 ) ) ;
#15437 = CARTESIAN_POINT ( 'NONE',  ( 85.53020504959901871, -140.9188050298377846, 60.00000000000000000 ) ) ;
#15438 = ORIENTED_EDGE ( 'NONE', *, *, #18017, .F. ) ;
#15439 = AXIS2_PLACEMENT_3D ( 'NONE', #19827, #1008, #14730 ) ;
#15440 = CIRCLE ( 'NONE', #9231, 3.224098631618460331 ) ;
#15441 = ORIENTED_EDGE ( 'NONE', *, *, #15533, .F. ) ;
#15442 = CARTESIAN_POINT ( 'NONE',  ( -97.70829847158753978, -133.6812691754211926, 32.03888873557544770 ) ) ;
#15443 = ORIENTED_EDGE ( 'NONE', *, *, #17624, .F. ) ;
#15444 = CARTESIAN_POINT ( 'NONE',  ( 9.564549117045078930, 62.18629025319817316, 132.4711112102474146 ) ) ;
#15445 = PLANE ( 'NONE',  #5659 ) ;
#15446 = CIRCLE ( 'NONE', #15795, 62.91752772691707207 ) ;
#15447 = ORIENTED_EDGE ( 'NONE', *, *, #14286, .F. ) ;
#15448 = AXIS2_PLACEMENT_3D ( 'NONE', #5482, #19403, #11705 ) ;
#15449 = CARTESIAN_POINT ( 'NONE',  ( 97.52076053070045702, -133.9271890290841611, 9.255816378659050159 ) ) ;
#15450 = CARTESIAN_POINT ( 'NONE',  ( 15.91767397667355510, 149.1530343478547422, 39.99999999999999289 ) ) ;
#15451 = AXIS2_PLACEMENT_3D ( 'NONE', #7237, #9171, #18181 ) ;
#15452 = DIRECTION ( 'NONE',  ( -0.1736481776669408228, -0.9848077530122062440, 2.152196535136390085E-15 ) ) ;
#15453 = EDGE_LOOP ( 'NONE', ( #4706, #532, #9303, #16821, #3560, #12536, #483, #15514 ) ) ;
#15454 = DIRECTION ( 'NONE',  ( 0.000000000000000000, -0.8660254037844380415, -0.5000000000000009992 ) ) ;
#15455 = DIRECTION ( 'NONE',  ( -1.000000000000000000, 0.000000000000000000, 0.000000000000000000 ) ) ;
#15456 = DIRECTION ( 'NONE',  ( 1.000000000000000000, 0.000000000000000000, 0.000000000000000000 ) ) ;
#15457 = CARTESIAN_POINT ( 'NONE',  ( 90.39157087502310617, -119.7120742831054372, 46.69505570264369254 ) ) ;
#15458 = ORIENTED_EDGE ( 'NONE', *, *, #2391, .F. ) ;
#15459 = CARTESIAN_POINT ( 'NONE',  ( -159.9599531637108782, -36.50981547337168109, 49.99999999999999289 ) ) ;
#15460 = DIRECTION ( 'NONE',  ( 0.3420201433256694901, -0.9396926207859082059, 0.000000000000000000 ) ) ;
#15461 = AXIS2_PLACEMENT_3D ( 'NONE', #19324, #5406, #14611 ) ;
#15462 = VECTOR ( 'NONE', #16193, 1000.000000000000000 ) ;
#15463 = EDGE_LOOP ( 'NONE', ( #7201, #9481, #5241, #17066 ) ) ;
#15464 = EDGE_CURVE ( 'NONE', #17279, #1274, #289, .T. ) ;
#15465 = VERTEX_POINT ( 'NONE', #387 ) ;
#15466 = SHAPE_DEFINITION_REPRESENTATION ( #9816, #17382 ) ;
#15467 = AXIS2_PLACEMENT_3D ( 'NONE', #7410, #4041, #8841 ) ;
#15468 = VERTEX_POINT ( 'NONE', #17590 ) ;
#15469 = LINE ( 'NONE', #12803, #8480 ) ;
#15470 = FACE_BOUND ( 'NONE', #3168, .T. ) ;
#15471 = VERTEX_POINT ( 'NONE', #6337 ) ;
#15472 = DIRECTION ( 'NONE',  ( -0.6155349844899689060, 0.7881095627315620744, 0.000000000000000000 ) ) ;
#15473 = LINE ( 'NONE', #6283, #15484 ) ;
#15474 = LINE ( 'NONE', #18138, #5837 ) ;
#15475 = CARTESIAN_POINT ( 'NONE',  ( 7.350000000000000533, 5.196152422706627583, 9.000000000000001776 ) ) ;
#15476 = ADVANCED_FACE ( 'NONE', ( #8257 ), #18248, .F. ) ;
#15477 = CARTESIAN_POINT ( 'NONE',  ( -96.59911734864401467, -114.8254675080908953, 36.23371386736513244 ) ) ;
#15478 = CARTESIAN_POINT ( 'NONE',  ( 71.18887634719571622, -147.8252249328912740, 39.99999999999999289 ) ) ;
#15479 = DIRECTION ( 'NONE',  ( 0.8830229359480271656, 0.4693298356057563625, 0.000000000000000000 ) ) ;
#15480 = EDGE_CURVE ( 'NONE', #19763, #12174, #5571, .T. ) ;
#15481 = CARTESIAN_POINT ( 'NONE',  ( -189.9999999999988916, 275.0000000000000000, 5.000000000000268230 ) ) ;
#15482 = CARTESIAN_POINT ( 'NONE',  ( -133.2712073792708907, -68.96827650320689429, 9.471058287156711941 ) ) ;
#15483 = CARTESIAN_POINT ( 'NONE',  ( 127.0298602564891013, -79.77387071031716914, -8.901236177966797669 ) ) ;
#15484 = VECTOR ( 'NONE', #6180, 1000.000000000000114 ) ;
#15485 = LINE ( 'NONE', #3010, #11147 ) ;
#15486 = CARTESIAN_POINT ( 'NONE',  ( -63.98537287693041264, 94.20918150411493741, 14.88498244535589876 ) ) ;
#15487 = CARTESIAN_POINT ( 'NONE',  ( -125.8775035253894146, -81.60755858752349923, 41.03713929422894324 ) ) ;
#15488 = ORIENTED_EDGE ( 'NONE', *, *, #4016, .T. ) ;
#15489 = DIRECTION ( 'NONE',  ( -1.000000000000000000, 0.000000000000000000, 0.000000000000000000 ) ) ;
#15490 = AXIS2_PLACEMENT_3D ( 'NONE', #18704, #19108, #1618 ) ;
#15491 = EDGE_CURVE ( 'NONE', #15722, #14388, #10933, .T. ) ;
#15492 = ORIENTED_EDGE ( 'NONE', *, *, #18527, .T. ) ;
#15493 = ORIENTED_EDGE ( 'NONE', *, *, #15392, .F. ) ;
#15494 = ORIENTED_EDGE ( 'NONE', *, *, #430, .T. ) ;
#15495 = AXIS2_PLACEMENT_3D ( 'NONE', #14331, #6566, #17512 ) ;
#15496 = CARTESIAN_POINT ( 'NONE',  ( -141.9821482856067689, -18.16655044785428075, -9.224423568343562252 ) ) ;
#15497 = CARTESIAN_POINT ( 'NONE',  ( -8.402595070145098433, -117.5408478153264298, 14.88498244535551152 ) ) ;
#15498 = EDGE_CURVE ( 'NONE', #3695, #17191, #13537, .T. ) ;
#15499 = VECTOR ( 'NONE', #1996, 1000.000000000000000 ) ;
#15500 = DIRECTION ( 'NONE',  ( -0.9902903945359624593, -0.1390141521205945918, 0.000000000000000000 ) ) ;
#15501 = ORIENTED_EDGE ( 'NONE', *, *, #14517, .T. ) ;
#15502 = EDGE_CURVE ( 'NONE', #1080, #13413, #16183, .T. ) ;
#15503 = CARTESIAN_POINT ( 'NONE',  ( -137.6581377289620320, -21.36537278083219604, -16.45265777907983917 ) ) ;
#15504 = CYLINDRICAL_SURFACE ( 'NONE', #4909, 62.91752772691707207 ) ;
#15505 = VERTEX_POINT ( 'NONE', #16621 ) ;
#15506 = CARTESIAN_POINT ( 'NONE',  ( -99.15300337306508993, 89.83204135164545789, -28.30778954837869676 ) ) ;
#15507 = PLANE ( 'NONE',  #2843 ) ;
#15508 = CARTESIAN_POINT ( 'NONE',  ( 97.50000000000002842, -189.9999999999999716, 10.00000000000000178 ) ) ;
#15509 = CARTESIAN_POINT ( 'NONE',  ( 0.000000000000000000, 0.000000000000000000, 132.4711112102474146 ) ) ;
#15510 = LINE ( 'NONE', #1496, #5579 ) ;
#15511 = DIRECTION ( 'NONE',  ( -0.6427876096865430267, 0.7660444431189749048, 0.000000000000000000 ) ) ;
#15512 = VECTOR ( 'NONE', #8732, 1000.000000000000114 ) ;
#15513 = CARTESIAN_POINT ( 'NONE',  ( -170.2125097089225960, -199.3942630591408260, 40.00000000000000000 ) ) ;
#15514 = ORIENTED_EDGE ( 'NONE', *, *, #3226, .F. ) ;
#15515 = VERTEX_POINT ( 'NONE', #13426 ) ;
#15516 = ADVANCED_FACE ( 'NONE', ( #19778 ), #1129, .F. ) ;
#15517 = ORIENTED_EDGE ( 'NONE', *, *, #1642, .T. ) ;
#15518 = EDGE_LOOP ( 'NONE', ( #13846, #17012, #15720, #1405 ) ) ;
#15519 = EDGE_CURVE ( 'NONE', #16556, #2269, #14605, .T. ) ;
#15520 = CARTESIAN_POINT ( 'NONE',  ( 60.68773558783009747, -2.629322876227576433, 293.5832628385307999 ) ) ;
#15521 = ORIENTED_EDGE ( 'NONE', *, *, #12135, .F. ) ;
#15522 = DIRECTION ( 'NONE',  ( -0.000000000000000000, -0.000000000000000000, 1.000000000000000000 ) ) ;
#15523 = VECTOR ( 'NONE', #10207, 1000.000000000000000 ) ;
#15524 = LINE ( 'NONE', #15729, #12696 ) ;
#15525 = DIRECTION ( 'NONE',  ( 0.9394263059140719463, 0.3427509529624103712, 0.000000000000000000 ) ) ;
#15526 = DIRECTION ( 'NONE',  ( -1.613511099790691498E-16, 1.000000000000000000, 0.000000000000000000 ) ) ;
#15527 = VERTEX_POINT ( 'NONE', #14970 ) ;
#15528 = EDGE_CURVE ( 'NONE', #9322, #2029, #12517, .T. ) ;
#15529 = AXIS2_PLACEMENT_3D ( 'NONE', #18978, #3419, #4962 ) ;
#15530 = EDGE_CURVE ( 'NONE', #16066, #12093, #8931, .T. ) ;
#15531 = CARTESIAN_POINT ( 'NONE',  ( -87.49999999999998579, -133.9542832461881687, 10.00000000000000000 ) ) ;
#15532 = CARTESIAN_POINT ( 'NONE',  ( -60.72073886220397299, 1.629865514042312613, 283.5832628385307999 ) ) ;
#15533 = EDGE_CURVE ( 'NONE', #19640, #10955, #587, .T. ) ;
#15534 = EDGE_CURVE ( 'NONE', #3447, #13254, #1157, .T. ) ;
#15535 = ORIENTED_EDGE ( 'NONE', *, *, #8308, .F. ) ;
#15536 = ADVANCED_FACE ( 'NONE', ( #7501 ), #18817, .F. ) ;
#15537 = DIRECTION ( 'NONE',  ( 0.000000000000000000, 0.000000000000000000, 1.000000000000000000 ) ) ;
#15538 = DIRECTION ( 'NONE',  ( 0.5000000000000069944, -0.8660254037844345998, 0.000000000000000000 ) ) ;
#15539 = DIRECTION ( 'NONE',  ( 1.000000000000000000, 0.000000000000000000, 0.000000000000000000 ) ) ;
#15540 = DIRECTION ( 'NONE',  ( -0.3427509529624101492, 0.9394263059140721683, 0.000000000000000000 ) ) ;
#15541 = DIRECTION ( 'NONE',  ( 1.000000000000000000, 0.000000000000000000, -6.994638739193269649E-15 ) ) ;
#15542 = AXIS2_PLACEMENT_3D ( 'NONE', #10206, #19619, #11734 ) ;
#15543 = CARTESIAN_POINT ( 'NONE',  ( -75.26415512511634631, 118.0479206960037288, 9.312873650067192699 ) ) ;
#15544 = ORIENTED_EDGE ( 'NONE', *, *, #1099, .F. ) ;
#15545 = DIRECTION ( 'NONE',  ( -1.000000000000000000, 0.000000000000000000, 0.000000000000000000 ) ) ;
#15546 = VERTEX_POINT ( 'NONE', #14754 ) ;
#15547 = VERTEX_POINT ( 'NONE', #9954 ) ;
#15548 = DIRECTION ( 'NONE',  ( -0.3747554100459959403, -0.9271237148521535021, 0.000000000000000000 ) ) ;
#15549 = VERTEX_POINT ( 'NONE', #8518 ) ;
#15550 = CARTESIAN_POINT ( 'NONE',  ( -147.0809924354783220, 29.44794838685322702, -9.999999999999978684 ) ) ;
#15551 = DIRECTION ( 'NONE',  ( 0.7660444431189726844, 0.6427876096865456912, 0.000000000000000000 ) ) ;
#15552 = ORIENTED_EDGE ( 'NONE', *, *, #8275, .F. ) ;
#15553 = ADVANCED_FACE ( 'NONE', ( #11484 ), #3713, .T. ) ;
#15554 = CARTESIAN_POINT ( 'NONE',  ( 97.70829847158759662, -133.6812691754159630, 7.961111264424513223 ) ) ;
#15555 = FACE_OUTER_BOUND ( 'NONE', #12207, .T. ) ;
#15556 = AXIS2_PLACEMENT_3D ( 'NONE', #17090, #3, #10939 ) ;
#15557 = EDGE_CURVE ( 'NONE', #15547, #12093, #646, .T. ) ;
#15558 = CARTESIAN_POINT ( 'NONE',  ( 7.500000000000420997, -60.00000000000000000, -105.0000000000000142 ) ) ;
#15559 = DIRECTION ( 'NONE',  ( -6.982962677686266711E-15, 0.000000000000000000, -1.000000000000000000 ) ) ;
#15560 = ORIENTED_EDGE ( 'NONE', *, *, #5237, .F. ) ;
#15561 = LINE ( 'NONE', #4719, #410 ) ;
#15562 = DIRECTION ( 'NONE',  ( -0.9396926207859092051, 0.3420201433256662704, 0.000000000000000000 ) ) ;
#15563 = CARTESIAN_POINT ( 'NONE',  ( -25.99419088092141550, 73.82206860051556419, 111.4180192758973931 ) ) ;
#15564 = CARTESIAN_POINT ( 'NONE',  ( 99.98138848894193131, -130.5820681961301375, 36.62898419040125475 ) ) ;
#15565 = CIRCLE ( 'NONE', #18171, 150.0000000000000284 ) ;
#15566 = ORIENTED_EDGE ( 'NONE', *, *, #6535, .F. ) ;
#15567 = CIRCLE ( 'NONE', #14897, 34.99999999999997868 ) ;
#15568 = CARTESIAN_POINT ( 'NONE',  ( 0.000000000000000000, 0.000000000000000000, 0.000000000000000000 ) ) ;
#15569 = CARTESIAN_POINT ( 'NONE',  ( 50.37374754117453080, -141.2886604036503115, 49.99999999999999289 ) ) ;
#15570 = ORIENTED_EDGE ( 'NONE', *, *, #14739, .T. ) ;
#15571 = EDGE_LOOP ( 'NONE', ( #6091, #15315 ) ) ;
#15572 = ORIENTED_EDGE ( 'NONE', *, *, #2102, .T. ) ;
#15573 = CARTESIAN_POINT ( 'NONE',  ( 0.000000000000000000, 0.000000000000000000, 0.000000000000000000 ) ) ;
#15574 = EDGE_LOOP ( 'NONE', ( #4113, #17027, #16431, #6940 ) ) ;
#15575 = DIRECTION ( 'NONE',  ( -0.000000000000000000, -0.000000000000000000, 1.000000000000000000 ) ) ;
#15576 = DIRECTION ( 'NONE',  ( -0.000000000000000000, -1.000000000000000000, -0.000000000000000000 ) ) ;
#15577 = ORIENTED_EDGE ( 'NONE', *, *, #19767, .T. ) ;
#15578 = CARTESIAN_POINT ( 'NONE',  ( 78.68887634719573043, -147.8252249328912740, 60.00000000000000000 ) ) ;
#15579 = DIRECTION ( 'NONE',  ( 6.982962677686266711E-15, -0.000000000000000000, 1.000000000000000000 ) ) ;
#15580 = CARTESIAN_POINT ( 'NONE',  ( -26.42151830275497915, 4.658826548058537576, 39.88498244535563941 ) ) ;
#15581 = VECTOR ( 'NONE', #2563, 1000.000000000000000 ) ;
#15582 = CARTESIAN_POINT ( 'NONE',  ( -95.87485967515243601, -116.0949201519087666, 30.54396691460070556 ) ) ;
#15583 = CARTESIAN_POINT ( 'NONE',  ( 0.000000000000000000, 0.000000000000000000, 0.000000000000000000 ) ) ;
#15584 = PLANE ( 'NONE',  #293 ) ;
#15585 = EDGE_CURVE ( 'NONE', #4629, #4234, #8213, .T. ) ;
#15586 = CYLINDRICAL_SURFACE ( 'NONE', #1309, 60.74260934110282051 ) ;
#15587 = DIRECTION ( 'NONE',  ( 0.8830229359480271656, 0.4693298356057563625, 0.000000000000000000 ) ) ;
#15588 = CIRCLE ( 'NONE', #9375, 7.500000000000002665 ) ;
#15589 = FACE_OUTER_BOUND ( 'NONE', #13428, .T. ) ;
#15590 = DIRECTION ( 'NONE',  ( -0.000000000000000000, -0.000000000000000000, 1.000000000000000000 ) ) ;
#15591 = FACE_OUTER_BOUND ( 'NONE', #2220, .T. ) ;
#15592 = CARTESIAN_POINT ( 'NONE',  ( -128.7754324793921228, -76.93177152330437707, 47.71976547401850866 ) ) ;
#15593 = ORIENTED_EDGE ( 'NONE', *, *, #19400, .T. ) ;
#15594 = DIRECTION ( 'NONE',  ( 0.9749279121818257288, -0.2225209339563047062, 0.000000000000000000 ) ) ;
#15595 = EDGE_CURVE ( 'NONE', #2786, #17433, #10945, .T. ) ;
#15596 = ORIENTED_EDGE ( 'NONE', *, *, #9444, .T. ) ;
#15597 = ORIENTED_EDGE ( 'NONE', *, *, #2523, .F. ) ;
#15598 = AXIS2_PLACEMENT_3D ( 'NONE', #9137, #1156, #17233 ) ;
#15599 = ORIENTED_EDGE ( 'NONE', *, *, #12660, .F. ) ;
#15600 = LINE ( 'NONE', #7916, #11887 ) ;
#15601 = CARTESIAN_POINT ( 'NONE',  ( -44.43084819159250287, 38.35506425062501989, 132.4711112102474146 ) ) ;
#15602 = ORIENTED_EDGE ( 'NONE', *, *, #12282, .F. ) ;
#15603 = DIRECTION ( 'NONE',  ( -0.9902903945359624593, -0.1390141521205945918, 0.000000000000000000 ) ) ;
#15604 = DIRECTION ( 'NONE',  ( 1.000000000000000000, 0.000000000000000000, 0.000000000000000000 ) ) ;
#15605 = ADVANCED_FACE ( 'NONE', ( #339 ), #19367, .F. ) ;
#15606 = LINE ( 'NONE', #6100, #8450 ) ;
#15607 = ADVANCED_FACE ( 'NONE', ( #5354 ), #3810, .F. ) ;
#15608 = LINE ( 'NONE', #1493, #14280 ) ;
#15609 = DIRECTION ( 'NONE',  ( 0.000000000000000000, 0.000000000000000000, 1.000000000000000000 ) ) ;
#15610 = CARTESIAN_POINT ( 'NONE',  ( 0.000000000000000000, -3.004629197474327134E-15, 9.000000000000000000 ) ) ;
#15611 = DIRECTION ( 'NONE',  ( -0.7660444431189862291, -0.6427876096865298150, 5.380491337840976593E-15 ) ) ;
#15612 = AXIS2_PLACEMENT_3D ( 'NONE', #16960, #10706, #20121 ) ;
#15613 = ORIENTED_EDGE ( 'NONE', *, *, #16859, .T. ) ;
#15614 = VECTOR ( 'NONE', #4306, 1000.000000000000114 ) ;
#15615 = CARTESIAN_POINT ( 'NONE',  ( -45.48770046196285932, -37.09555676056982065, 110.7293897666001214 ) ) ;
#15616 = DIRECTION ( 'NONE',  ( 0.000000000000000000, 0.000000000000000000, 1.000000000000000000 ) ) ;
#15617 = ORIENTED_EDGE ( 'NONE', *, *, #6787, .F. ) ;
#15618 = ORIENTED_EDGE ( 'NONE', *, *, #12081, .T. ) ;
#15619 = ADVANCED_FACE ( 'NONE', ( #551 ), #16001, .T. ) ;
#15620 = ORIENTED_EDGE ( 'NONE', *, *, #15013, .T. ) ;
#15621 = ADVANCED_FACE ( 'NONE', ( #17446, #17643 ), #19078, .T. ) ;
#15622 = ORIENTED_EDGE ( 'NONE', *, *, #376, .T. ) ;
#15623 = EDGE_CURVE ( 'NONE', #5786, #5586, #11912, .T. ) ;
#15624 = DIRECTION ( 'NONE',  ( 0.000000000000000000, 0.000000000000000000, -1.000000000000000000 ) ) ;
#15625 = ORIENTED_EDGE ( 'NONE', *, *, #4532, .T. ) ;
#15626 = DIRECTION ( 'NONE',  ( 0.000000000000000000, 1.000000000000000000, 0.000000000000000000 ) ) ;
#15627 = CONICAL_SURFACE ( 'NONE', #5824, 5.035999999999999588, 0.7853981633974425058 ) ;
#15628 = CARTESIAN_POINT ( 'NONE',  ( -97.53506906366366991, -133.9085396777615244, 30.96104885487609337 ) ) ;
#15629 = CARTESIAN_POINT ( 'NONE',  ( 0.000000000000000000, 0.000000000000000000, 60.00000000000000000 ) ) ;
#15630 = AXIS2_PLACEMENT_3D ( 'NONE', #15976, #8291, #4941 ) ;
#15631 = CARTESIAN_POINT ( 'NONE',  ( -109.9999999999983515, 275.0000000000000000, 85.00000000000001421 ) ) ;
#15632 = CARTESIAN_POINT ( 'NONE',  ( -109.5721339228237667, 31.03941509555038181, 14.88498244535621851 ) ) ;
#15633 = EDGE_LOOP ( 'NONE', ( #11159, #7408, #12329, #3675 ) ) ;
#15634 = CYLINDRICAL_SURFACE ( 'NONE', #3795, 62.91752772691707207 ) ;
#15635 = CARTESIAN_POINT ( 'NONE',  ( 53.40245231972179596, 28.94983032429848535, 293.5832628385307999 ) ) ;
#15636 = ADVANCED_FACE ( 'NONE', ( #5064 ), #9649, .T. ) ;
#15637 = ORIENTED_EDGE ( 'NONE', *, *, #9530, .F. ) ;
#15638 = PRODUCT_DEFINITION_CONTEXT ( 'detailed design', #453, 'design' ) ;
#15639 = CARTESIAN_POINT ( 'NONE',  ( -79.24532193214523090, 125.6874967381585435, -20.60241429600958085 ) ) ;
#15640 = CARTESIAN_POINT ( 'NONE',  ( 0.000000000000000000, 0.000000000000000000, 283.5832628385307999 ) ) ;
#15641 = DIRECTION ( 'NONE',  ( 1.000000000000000000, 0.000000000000000000, 0.000000000000000000 ) ) ;
#15642 = AXIS2_PLACEMENT_3D ( 'NONE', #18394, #7435, #4167 ) ;
#15643 = LINE ( 'NONE', #14097, #2527 ) ;
#15644 = LINE ( 'NONE', #1632, #13720 ) ;
#15645 = CARTESIAN_POINT ( 'NONE',  ( -104.5696057486236441, 93.10197836950014505, 39.59507579059730631 ) ) ;
#15646 = VECTOR ( 'NONE', #752, 1000.000000000000000 ) ;
#15647 = AXIS2_PLACEMENT_3D ( 'NONE', #14527, #14720, #13269 ) ;
#15648 = VERTEX_POINT ( 'NONE', #6594 ) ;
#15649 = CIRCLE ( 'NONE', #14985, 7.500000000000020428 ) ;
#15650 = DIRECTION ( 'NONE',  ( 0.000000000000000000, 0.000000000000000000, -1.000000000000000000 ) ) ;
#15651 = ORIENTED_EDGE ( 'NONE', *, *, #5782, .F. ) ;
#15652 = EDGE_CURVE ( 'NONE', #9808, #20114, #8336, .T. ) ;
#15653 = EDGE_CURVE ( 'NONE', #4680, #13974, #5258, .T. ) ;
#15654 = ORIENTED_EDGE ( 'NONE', *, *, #10120, .T. ) ;
#15655 = ADVANCED_FACE ( 'NONE', ( #448 ), #2147, .T. ) ;
#15656 = LINE ( 'NONE', #17192, #16312 ) ;
#15657 = ORIENTED_EDGE ( 'NONE', *, *, #964, .F. ) ;
#15658 = CARTESIAN_POINT ( 'NONE',  ( -117.9669857229114314, 78.77317465270277808, -34.20188040274583585 ) ) ;
#15659 = FACE_OUTER_BOUND ( 'NONE', #2791, .T. ) ;
#15660 = ORIENTED_EDGE ( 'NONE', *, *, #2895, .T. ) ;
#15661 = CARTESIAN_POINT ( 'NONE',  ( 85.13411715130894208, -123.5004392096819146, -1.042466200307516466 ) ) ;
#15662 = LINE ( 'NONE', #10831, #13207 ) ;
#15663 = VECTOR ( 'NONE', #2226, 1000.000000000000000 ) ;
#15664 = EDGE_CURVE ( 'NONE', #10905, #2341, #19764, .T. ) ;
#15665 = CARTESIAN_POINT ( 'NONE',  ( -103.8888757476053541, -46.65403860089418941, 14.88498244535617765 ) ) ;
#15666 = SURFACE_STYLE_FILL_AREA ( #15345 ) ;
#15667 = ORIENTED_EDGE ( 'NONE', *, *, #3690, .F. ) ;
#15668 = LINE ( 'NONE', #6263, #2369 ) ;
#15669 = FACE_OUTER_BOUND ( 'NONE', #9214, .T. ) ;
#15670 = DIRECTION ( 'NONE',  ( 6.982962677686266711E-15, -0.000000000000000000, 1.000000000000000000 ) ) ;
#15671 = CARTESIAN_POINT ( 'NONE',  ( 96.12039245754215244, -116.0188909747135853, 30.17258640897478372 ) ) ;
#15672 = EDGE_LOOP ( 'NONE', ( #10198, #15060, #2916, #13310 ) ) ;
#15673 = LINE ( 'NONE', #11054, #18910 ) ;
#15674 = CARTESIAN_POINT ( 'NONE',  ( -87.64225943403401686, 121.7426507922284600, 38.20596441781194130 ) ) ;
#15675 = EDGE_CURVE ( 'NONE', #3202, #17939, #18722, .T. ) ;
#15676 = EDGE_CURVE ( 'NONE', #6317, #18284, #2577, .T. ) ;
#15677 = EDGE_LOOP ( 'NONE', ( #7937, #5334, #3466, #18887, #2191 ) ) ;
#15678 = VECTOR ( 'NONE', #8797, 1000.000000000000000 ) ;
#15679 = AXIS2_PLACEMENT_3D ( 'NONE', #3130, #7716, #4449 ) ;
#15680 = ORIENTED_EDGE ( 'NONE', *, *, #9915, .F. ) ;
#15681 = ORIENTED_EDGE ( 'NONE', *, *, #14248, .T. ) ;
#15682 = DIRECTION ( 'NONE',  ( 0.000000000000000000, 0.000000000000000000, 1.000000000000000000 ) ) ;
#15683 = VERTEX_POINT ( 'NONE', #4002 ) ;
#15684 = EDGE_CURVE ( 'NONE', #8543, #2811, #14139, .T. ) ;
#15685 = CARTESIAN_POINT ( 'NONE',  ( -97.50000000000000000, -133.9542832461881972, 9.514131777208458374 ) ) ;
#15686 = CARTESIAN_POINT ( 'NONE',  ( -29.99999999999887379, 285.0000000000000568, 4.999999999999158007 ) ) ;
#15687 = ORIENTED_EDGE ( 'NONE', *, *, #4482, .T. ) ;
#15688 = DIRECTION ( 'NONE',  ( 0.4338837391175662250, -0.9009688679024151492, 0.000000000000000000 ) ) ;
#15689 = DIRECTION ( 'NONE',  ( 0.000000000000000000, 0.000000000000000000, -1.000000000000000000 ) ) ;
#15690 = FACE_OUTER_BOUND ( 'NONE', #13796, .T. ) ;
#15691 = B_SPLINE_CURVE_WITH_KNOTS ( 'NONE', 3,
 ( #8367, #5307, #593, #7040, #19609, #15003 ),
 .UNSPECIFIED., .F., .F.,
 ( 4, 2, 4 ),
 ( 0.03045342003272952236, 0.03308352805739833702, 0.03571363608206715862 ),
 .UNSPECIFIED. ) ;
#15692 = CARTESIAN_POINT ( 'NONE',  ( -103.0319911124590533, -126.0382377111977377, 38.95151328076024555 ) ) ;
#15693 = CARTESIAN_POINT ( 'NONE',  ( -156.4179374840092862, -52.02840013024096066, 39.99999999999999289 ) ) ;
#15694 = LINE ( 'NONE', #6589, #15350 ) ;
#15695 = CYLINDRICAL_SURFACE ( 'NONE', #9867, 7.500000000000007105 ) ;
#15696 = DIRECTION ( 'NONE',  ( -0.000000000000000000, -0.000000000000000000, 1.000000000000000000 ) ) ;
#15697 = CARTESIAN_POINT ( 'NONE',  ( 27.53920554013639688, 73.25972925305639194, 111.4180192758974499 ) ) ;
#15698 = CARTESIAN_POINT ( 'NONE',  ( -133.8370531740368108, -67.73246766859803358, 39.14630742583677403 ) ) ;
#15699 = ORIENTED_EDGE ( 'NONE', *, *, #1658, .T. ) ;
#15700 = PRODUCT ( 'Upper Flange', 'Upper Flange', '', ( #1971 ) ) ;
#15701 = DIRECTION ( 'NONE',  ( -0.000000000000000000, -0.000000000000000000, 1.000000000000000000 ) ) ;
#15702 = AXIS2_PLACEMENT_3D ( 'NONE', #11153, #3391, #15873 ) ;
#15703 = ORIENTED_EDGE ( 'NONE', *, *, #555, .F. ) ;
#15704 = AXIS2_PLACEMENT_3D ( 'NONE', #18839, #9521, #14118 ) ;
#15705 = ORIENTED_EDGE ( 'NONE', *, *, #14355, .T. ) ;
#15706 = EDGE_LOOP ( 'NONE', ( #12744, #5738, #19468, #6011 ) ) ;
#15707 = CARTESIAN_POINT ( 'NONE',  ( -144.4627684701566466, -14.76432773141799260, -1.188257704013451654 ) ) ;
#15708 = CARTESIAN_POINT ( 'NONE',  ( 68.18670162478805707, 38.41834839689404646, 132.4711112102474146 ) ) ;
#15709 = CARTESIAN_POINT ( 'NONE',  ( 40.32479851956816930, -67.08601213326551260, 248.9926560891072143 ) ) ;
#15710 = LINE ( 'NONE', #9047, #18281 ) ;
#15711 = LINE ( 'NONE', #8128, #296 ) ;
#15712 = PLANE ( 'NONE',  #11503 ) ;
#15713 = DIRECTION ( 'NONE',  ( 0.000000000000000000, 0.000000000000000000, -1.000000000000000000 ) ) ;
#15714 = LINE ( 'NONE', #1696, #10461 ) ;
#15715 = CARTESIAN_POINT ( 'NONE',  ( 0.000000000000000000, 0.000000000000000000, 132.4711112102474146 ) ) ;
#15716 = ORIENTED_EDGE ( 'NONE', *, *, #987, .T. ) ;
#15717 = CARTESIAN_POINT ( 'NONE',  ( -7.500000000000006217, 164.0736214083062805, 39.99999999999999289 ) ) ;
#15718 = LINE ( 'NONE', #5848, #6093 ) ;
#15719 = ORIENTED_EDGE ( 'NONE', *, *, #5735, .T. ) ;
#15720 = ORIENTED_EDGE ( 'NONE', *, *, #5068, .T. ) ;
#15721 = VERTEX_POINT ( 'NONE', #8903 ) ;
#15722 = VERTEX_POINT ( 'NONE', #5646 ) ;
#15723 = EDGE_CURVE ( 'NONE', #9758, #15949, #17938, .T. ) ;
#15724 = FACE_OUTER_BOUND ( 'NONE', #13345, .T. ) ;
#15725 = AXIS2_PLACEMENT_3D ( 'NONE', #16944, #6104, #7828 ) ;
#15726 = ORIENTED_EDGE ( 'NONE', *, *, #7717, .F. ) ;
#15727 = DIRECTION ( 'NONE',  ( -0.9396926207859127578, 0.3420201433256568335, 0.000000000000000000 ) ) ;
#15728 = CARTESIAN_POINT ( 'NONE',  ( 59.42266395395792955, -50.93469132750283279, 110.7293897666001214 ) ) ;
#15729 = CARTESIAN_POINT ( 'NONE',  ( 2.605298826210328045, 5.111158570922230915, 293.5832628385307999 ) ) ;
#15730 = CARTESIAN_POINT ( 'NONE',  ( -189.9999999999988916, 265.0000000000000000, -2.499999999999734879 ) ) ;
#15731 = EDGE_LOOP ( 'NONE', ( #5102, #17962, #619, #17743 ) ) ;
#15732 = CARTESIAN_POINT ( 'NONE',  ( 7.350000000000001421, -7.794228634059948035, -4.499999999999999112 ) ) ;
#15733 = DIRECTION ( 'NONE',  ( 1.000000000000000000, 0.000000000000000000, 0.000000000000000000 ) ) ;
#15734 = EDGE_LOOP ( 'NONE', ( #9830, #4974 ) ) ;
#15735 = EDGE_CURVE ( 'NONE', #3219, #19783, #16427, .T. ) ;
#15736 = DIRECTION ( 'NONE',  ( -0.000000000000000000, -0.000000000000000000, -1.000000000000000000 ) ) ;
#15737 = LINE ( 'NONE', #13888, #9437 ) ;
#15738 = ADVANCED_FACE ( 'NONE', ( #8613 ), #18223, .T. ) ;
#15739 = EDGE_CURVE ( 'NONE', #3073, #15683, #1132, .T. ) ;
#15740 = DIRECTION ( 'NONE',  ( -0.5000000000000039968, 0.8660254037844363761, 0.000000000000000000 ) ) ;
#15741 = CYLINDRICAL_SURFACE ( 'NONE', #15264, 9.999999999999998224 ) ;
#15742 = DIRECTION ( 'NONE',  ( -0.9781142164131917394, 0.2080686897406911207, 0.000000000000000000 ) ) ;
#15743 = CARTESIAN_POINT ( 'NONE',  ( -75.81749350294444412, 117.6933339947108976, -2.532388154262697810 ) ) ;
#15744 = B_SPLINE_CURVE_WITH_KNOTS ( 'NONE', 3,
 ( #7949, #12552, #3353, #3258, #9592, #1514 ),
 .UNSPECIFIED., .F., .F.,
 ( 4, 2, 4 ),
 ( 2.380730968235596737E-07, 0.002629065763328352658, 0.005257893453559881955 ),
 .UNSPECIFIED. ) ;
#15745 = ORIENTED_EDGE ( 'NONE', *, *, #242, .F. ) ;
#15746 = LINE ( 'NONE', #6549, #2395 ) ;
#15747 = ORIENTED_EDGE ( 'NONE', *, *, #15413, .T. ) ;
#15748 = ORIENTED_EDGE ( 'NONE', *, *, #16795, .T. ) ;
#15749 = ADVANCED_FACE ( 'NONE', ( #7372 ), #15051, .T. ) ;
#15750 = CARTESIAN_POINT ( 'NONE',  ( -110.0000000000000142, 285.0000000000000568, -82.50000000000001421 ) ) ;
#15751 = ORIENTED_EDGE ( 'NONE', *, *, #157, .F. ) ;
#15752 = DIRECTION ( 'NONE',  ( 0.000000000000000000, 1.000000000000000000, -0.000000000000000000 ) ) ;
#15753 = FACE_BOUND ( 'NONE', #13064, .T. ) ;
#15754 = VERTEX_POINT ( 'NONE', #11964 ) ;
#15755 =( NAMED_UNIT ( * ) PLANE_ANGLE_UNIT ( ) SI_UNIT ( $, .RADIAN. ) );
#15756 = DIRECTION ( 'NONE',  ( -1.000000000000000000, 0.000000000000000000, 0.000000000000000000 ) ) ;
#15757 = EDGE_CURVE ( 'NONE', #10035, #18230, #14945, .T. ) ;
#15758 = AXIS2_PLACEMENT_3D ( 'NONE', #18355, #20191, #17029 ) ;
#15759 = AXIS2_PLACEMENT_3D ( 'NONE', #3133, #2826, #4669 ) ;
#15760 = EDGE_CURVE ( 'NONE', #5114, #4761, #7277, .T. ) ;
#15761 = EDGE_CURVE ( 'NONE', #10905, #16353, #16692, .T. ) ;
#15762 = DIRECTION ( 'NONE',  ( 1.000000000000000000, 0.000000000000000000, -6.976128451377902853E-15 ) ) ;
#15763 = CARTESIAN_POINT ( 'NONE',  ( 60.22029172860436574, 7.948651060879242003, 293.5832628385307999 ) ) ;
#15764 = ORIENTED_EDGE ( 'NONE', *, *, #5928, .F. ) ;
#15765 = DIRECTION ( 'NONE',  ( 1.000000000000000000, 0.000000000000000000, 0.000000000000000000 ) ) ;
#15766 = CARTESIAN_POINT ( 'NONE',  ( 0.000000000000000000, 0.000000000000000000, 132.4711112102474146 ) ) ;
#15767 = LINE ( 'NONE', #15973, #16354 ) ;
#15768 = FACE_BOUND ( 'NONE', #14838, .T. ) ;
#15769 = ORIENTED_EDGE ( 'NONE', *, *, #6281, .F. ) ;
#15770 = DIRECTION ( 'NONE',  ( 1.000000000000000000, 0.000000000000000000, 0.000000000000000000 ) ) ;
#15771 = CARTESIAN_POINT ( 'NONE',  ( -93.64123074234042576, 117.1838922457435217, 41.50921557003555051 ) ) ;
#15772 = ORIENTED_EDGE ( 'NONE', *, *, #12233, .T. ) ;
#15773 = VERTEX_POINT ( 'NONE', #933 ) ;
#15774 = EDGE_LOOP ( 'NONE', ( #10134, #16899 ) ) ;
#15775 = EDGE_CURVE ( 'NONE', #6744, #1994, #7186, .T. ) ;
#15776 = DIRECTION ( 'NONE',  ( 1.000000000000000000, 0.000000000000000000, 0.000000000000000000 ) ) ;
#15777 = VECTOR ( 'NONE', #342, 1000.000000000000000 ) ;
#15778 = EDGE_LOOP ( 'NONE', ( #7126, #3370, #8392 ) ) ;
#15779 = CARTESIAN_POINT ( 'NONE',  ( -1.396592535537253342E-14, 0.000000000000000000, 39.88498244535545467 ) ) ;
#15780 = DIRECTION ( 'NONE',  ( -0.9271237148521547233, 0.3747554100459928872, 0.000000000000000000 ) ) ;
#15781 = ORIENTED_EDGE ( 'NONE', *, *, #3649, .T. ) ;
#15782 = VECTOR ( 'NONE', #832, 1000.000000000000000 ) ;
#15783 = DIRECTION ( 'NONE',  ( -0.000000000000000000, -0.000000000000000000, -1.000000000000000000 ) ) ;
#15784 = DIRECTION ( 'NONE',  ( 0.6427876096865405842, -0.7660444431189771253, 0.000000000000000000 ) ) ;
#15785 = DIRECTION ( 'NONE',  ( 0.000000000000000000, 0.000000000000000000, 1.000000000000000000 ) ) ;
#15786 = CARTESIAN_POINT ( 'NONE',  ( -96.12355554546984138, -116.0165654454242485, 30.18179740741101114 ) ) ;
#15787 = EDGE_CURVE ( 'NONE', #19280, #13684, #2784, .T. ) ;
#15788 = DIRECTION ( 'NONE',  ( 1.000000000000000000, 0.000000000000000000, 0.000000000000000000 ) ) ;
#15789 = EDGE_CURVE ( 'NONE', #9422, #17872, #10334, .T. ) ;
#15790 = ADVANCED_FACE ( 'NONE', ( #12065 ), #16592, .T. ) ;
#15791 = CARTESIAN_POINT ( 'NONE',  ( -92.21618480002783258, -118.3073397699786540, -7.802271786604253023 ) ) ;
#15792 = CARTESIAN_POINT ( 'NONE',  ( 107.5000000000000142, -118.5063289449133492, 0.000000000000000000 ) ) ;
#15793 = CARTESIAN_POINT ( 'NONE',  ( 77.50000000000000000, 0.000000000000000000, -115.0000000000000000 ) ) ;
#15794 = CARTESIAN_POINT ( 'NONE',  ( 0.000000000000000000, 0.000000000000000000, 132.4711112102474146 ) ) ;
#15795 = AXIS2_PLACEMENT_3D ( 'NONE', #13715, #5957, #4413 ) ;
#15796 = AXIS2_PLACEMENT_3D ( 'NONE', #4635, #10859, #6380 ) ;
#15797 = DIRECTION ( 'NONE',  ( -0.000000000000000000, -0.000000000000000000, 1.000000000000000000 ) ) ;
#15798 = CARTESIAN_POINT ( 'NONE',  ( -3.911853314815649796, 4.196299268919085890, 283.5832628385307999 ) ) ;
#15799 = CARTESIAN_POINT ( 'NONE',  ( -130.9519479124771237, -73.15688856708418086, 45.28395117799519909 ) ) ;
#15800 = VERTEX_POINT ( 'NONE', #19466 ) ;
#15801 = CARTESIAN_POINT ( 'NONE',  ( 0.000000000000000000, 0.000000000000000000, 283.5832628385307999 ) ) ;
#15802 = EDGE_CURVE ( 'NONE', #2793, #12901, #14776, .T. ) ;
#15803 = VECTOR ( 'NONE', #2943, 1000.000000000000000 ) ;
#15804 = ORIENTED_EDGE ( 'NONE', *, *, #10505, .T. ) ;
#15805 = ORIENTED_EDGE ( 'NONE', *, *, #5735, .F. ) ;
#15806 = AXIS2_PLACEMENT_3D ( 'NONE', #1831, #15950, #6446 ) ;
#15807 = EDGE_LOOP ( 'NONE', ( #20091, #19492, #17762, #12263 ) ) ;
#15808 = FACE_OUTER_BOUND ( 'NONE', #5931, .T. ) ;
#15809 = CARTESIAN_POINT ( 'NONE',  ( 58.03804081968166173, -8.833100819207778898, 112.0427633081292385 ) ) ;
#15810 = CIRCLE ( 'NONE', #15467, 40.00000000000000711 ) ;
#15811 = DIRECTION ( 'NONE',  ( 0.8660254037844432595, -0.4999999999999919509, 0.000000000000000000 ) ) ;
#15812 = ORIENTED_EDGE ( 'NONE', *, *, #11469, .F. ) ;
#15813 = DIRECTION ( 'NONE',  ( 0.000000000000000000, 0.000000000000000000, 1.000000000000000000 ) ) ;
#15814 = CARTESIAN_POINT ( 'NONE',  ( 128.2779226595531270, 102.2982297021113141, 49.99999999999999289 ) ) ;
#15815 = LINE ( 'NONE', #12629, #19260 ) ;
#15816 = VECTOR ( 'NONE', #378, 1000.000000000000000 ) ;
#15817 = CARTESIAN_POINT ( 'NONE',  ( 97.77474281578807336, -133.5937942518637556, 32.33949703673819442 ) ) ;
#15818 = DIRECTION ( 'NONE',  ( -1.000000000000000000, 0.000000000000000000, 0.000000000000000000 ) ) ;
#15819 = EDGE_CURVE ( 'NONE', #20066, #19327, #10151, .T. ) ;
#15820 = ORIENTED_EDGE ( 'NONE', *, *, #9660, .F. ) ;
#15821 = SHAPE_REPRESENTATION ( 'hex bolt gradec_iso_ISO 4016 - M12 x 55 x 30-WN', ( #18639 ), #2627 ) ;
#15822 = CARTESIAN_POINT ( 'NONE',  ( 135.1060089022256818, -65.16414933467420667, 30.00000000000000000 ) ) ;
#15823 = CARTESIAN_POINT ( 'NONE',  ( 133.9050245804181998, -78.55577302928909944, 36.83190385597256977 ) ) ;
#15824 = ORIENTED_EDGE ( 'NONE', *, *, #12864, .T. ) ;
#15825 = ORIENTED_EDGE ( 'NONE', *, *, #4242, .F. ) ;
#15826 = ORIENTED_EDGE ( 'NONE', *, *, #4535, .F. ) ;
#15827 = VECTOR ( 'NONE', #17831, 1000.000000000000000 ) ;
#15828 = EDGE_LOOP ( 'NONE', ( #8015, #19285 ) ) ;
#15829 = CARTESIAN_POINT ( 'NONE',  ( -67.50000000000000000, -2.085703952312275003E-13, -115.0000000000000000 ) ) ;
#15830 = VECTOR ( 'NONE', #17556, 1000.000000000000000 ) ;
#15831 = ORIENTED_EDGE ( 'NONE', *, *, #8359, .F. ) ;
#15832 = FACE_OUTER_BOUND ( 'NONE', #15988, .T. ) ;
#15833 = CARTESIAN_POINT ( 'NONE',  ( -97.63639055817483836, -133.7757280588254218, 31.66285136016151114 ) ) ;
#15834 = CARTESIAN_POINT ( 'NONE',  ( 28.06680738835026290, -53.87178215532764369, 293.5832628385307999 ) ) ;
#15835 = PLANE ( 'NONE',  #1886 ) ;
#15836 = VERTEX_POINT ( 'NONE', #17207 ) ;
#15837 = CARTESIAN_POINT ( 'NONE',  ( 0.000000000000000000, 0.000000000000000000, 49.99999999999999289 ) ) ;
#15838 = CARTESIAN_POINT ( 'NONE',  ( 0.000000000000000000, 0.000000000000000000, -40.00000000000000000 ) ) ;
#15839 = ORIENTED_EDGE ( 'NONE', *, *, #4482, .F. ) ;
#15840 = LINE ( 'NONE', #384, #8390 ) ;
#15841 = PLANE ( 'NONE',  #3244 ) ;
#15842 = AXIS2_PLACEMENT_3D ( 'NONE', #5845, #11764, #7272 ) ;
#15843 = CARTESIAN_POINT ( 'NONE',  ( 55.16472960512370349, -30.25670013172234007, 293.5832628385307999 ) ) ;
#15844 = ADVANCED_FACE ( 'NONE', ( #11052 ), #20231, .F. ) ;
#15845 = DIRECTION ( 'NONE',  ( -0.9511061040868794558, -0.3088643371590157338, 0.000000000000000000 ) ) ;
#15846 = DIRECTION ( 'NONE',  ( 0.000000000000000000, 0.000000000000000000, 1.000000000000000000 ) ) ;
#15847 = DIRECTION ( 'NONE',  ( 1.000000000000000000, 0.000000000000000000, 0.000000000000000000 ) ) ;
#15848 = FACE_OUTER_BOUND ( 'NONE', #1277, .T. ) ;
#15849 = ORIENTED_EDGE ( 'NONE', *, *, #17560, .F. ) ;
#15850 = CARTESIAN_POINT ( 'NONE',  ( 58.83691981461633702, -22.28973221005102090, 248.9926560891072143 ) ) ;
#15851 = ORIENTED_EDGE ( 'NONE', *, *, #19711, .F. ) ;
#15852 = CIRCLE ( 'NONE', #12613, 10.00000000000000888 ) ;
#15853 = ORIENTED_EDGE ( 'NONE', *, *, #15595, .F. ) ;
#15854 = DIRECTION ( 'NONE',  ( 0.000000000000000000, 0.000000000000000000, -1.000000000000000000 ) ) ;
#15855 = EDGE_CURVE ( 'NONE', #8838, #14482, #11560, .T. ) ;
#15856 = AXIS2_PLACEMENT_3D ( 'NONE', #5006, #2034, #3564 ) ;
#15857 = ORIENTED_EDGE ( 'NONE', *, *, #3793, .T. ) ;
#15858 = CARTESIAN_POINT ( 'NONE',  ( -143.0849254817002816, 42.75236248750393031, -17.56505644796369126 ) ) ;
#15859 = DIRECTION ( 'NONE',  ( 0.000000000000000000, 0.000000000000000000, 1.000000000000000000 ) ) ;
#15860 = VERTEX_POINT ( 'NONE', #17517 ) ;
#15861 = SURFACE_STYLE_FILL_AREA ( #9813 ) ;
#15862 = FACE_OUTER_BOUND ( 'NONE', #17947, .T. ) ;
#15863 = DIRECTION ( 'NONE',  ( -1.000000000000000000, 0.000000000000000000, 0.000000000000000000 ) ) ;
#15864 = PRODUCT_DEFINITION_SHAPE ( 'NONE', 'NONE',  #8394 ) ;
#15865 = AXIS2_PLACEMENT_3D ( 'NONE', #17802, #16269, #2249 ) ;
#15866 = EDGE_CURVE ( 'NONE', #16460, #541, #12689, .T. ) ;
#15867 = CARTESIAN_POINT ( 'NONE',  ( -59.58067424803613221, 20.21777810286735289, 248.9926560891072143 ) ) ;
#15868 = DIRECTION ( 'NONE',  ( 0.000000000000000000, 0.000000000000000000, 1.000000000000000000 ) ) ;
#15869 = ORIENTED_EDGE ( 'NONE', *, *, #3649, .F. ) ;
#15870 = CARTESIAN_POINT ( 'NONE',  ( -30.74413178637153976, 54.89456854707572830, 248.9926560891072143 ) ) ;
#15871 = APPLICATION_CONTEXT ( 'automotive_design' ) ;
#15872 = DIRECTION ( 'NONE',  ( -6.982962677686266711E-15, 0.000000000000000000, -1.000000000000000000 ) ) ;
#15873 = DIRECTION ( 'NONE',  ( 1.000000000000000000, 0.000000000000000000, 0.000000000000000000 ) ) ;
#15874 = DIRECTION ( 'NONE',  ( 8.659560562354966138E-17, 0.7071067811865447972, -0.7071067811865502373 ) ) ;
#15875 = ORIENTED_EDGE ( 'NONE', *, *, #13472, .F. ) ;
#15876 = CARTESIAN_POINT ( 'NONE',  ( 42.50000000000000000, 0.000000000000000000, -49.99999999999999289 ) ) ;
#15877 = DIRECTION ( 'NONE',  ( -1.000000000000000000, -0.000000000000000000, 0.000000000000000000 ) ) ;
#15878 = VERTEX_POINT ( 'NONE', #11361 ) ;
#15879 = VECTOR ( 'NONE', #2225, 1000.000000000000227 ) ;
#15880 = ORIENTED_EDGE ( 'NONE', *, *, #9145, .T. ) ;
#15881 = VERTEX_POINT ( 'NONE', #14632 ) ;
#15882 = EDGE_CURVE ( 'NONE', #5311, #15357, #3489, .T. ) ;
#15883 = AXIS2_PLACEMENT_3D ( 'NONE', #2444, #13263, #8674 ) ;
#15884 = ORIENTED_EDGE ( 'NONE', *, *, #18673, .F. ) ;
#15885 = EDGE_CURVE ( 'NONE', #17837, #3073, #522, .T. ) ;
#15886 = CARTESIAN_POINT ( 'NONE',  ( 0.000000000000000000, 0.000000000000000000, -39.99999999999999289 ) ) ;
#15887 = CARTESIAN_POINT ( 'NONE',  ( -150.0000000000000000, 0.000000000000000000, 5.000000000000011546 ) ) ;
#15888 = VERTEX_POINT ( 'NONE', #8190 ) ;
#15889 = CARTESIAN_POINT ( 'NONE',  ( -109.5721339228235820, 31.03941509555038181, 39.88498244535622206 ) ) ;
#15890 = CARTESIAN_POINT ( 'NONE',  ( 126.7590367374603346, -80.21250349114239953, 49.07649135601570123 ) ) ;
#15891 = CIRCLE ( 'NONE', #5435, 106.4288957539801288 ) ;
#15892 = CARTESIAN_POINT ( 'NONE',  ( -100.2452644940503177, -111.5858889953167790, -10.00000000000000000 ) ) ;
#15893 = DIRECTION ( 'NONE',  ( 0.8660254037844415942, -0.4999999999999950040, 0.000000000000000000 ) ) ;
#15894 = EDGE_CURVE ( 'NONE', #6700, #20169, #1390, .T. ) ;
#15895 = CARTESIAN_POINT ( 'NONE',  ( -147.0809924354783220, 29.44794838685322702, -9.999999999999978684 ) ) ;
#15896 = FACE_OUTER_BOUND ( 'NONE', #6198, .T. ) ;
#15897 = DIRECTION ( 'NONE',  ( 0.000000000000000000, 0.000000000000000000, 1.000000000000000000 ) ) ;
#15898 = DIRECTION ( 'NONE',  ( -0.000000000000000000, -0.000000000000000000, 1.000000000000000000 ) ) ;
#15899 = VERTEX_POINT ( 'NONE', #13085 ) ;
#15900 = CARTESIAN_POINT ( 'NONE',  ( -111.9190551610216744, 70.74871087183512941, -30.00000000000067146 ) ) ;
#15901 = ORIENTED_EDGE ( 'NONE', *, *, #6814, .T. ) ;
#15902 = ADVANCED_FACE ( 'NONE', ( #2065 ), #19250, .F. ) ;
#15903 = CIRCLE ( 'NONE', #6435, 7.500000000000007105 ) ;
#15904 = EDGE_LOOP ( 'NONE', ( #8369, #424 ) ) ;
#15905 = EDGE_CURVE ( 'NONE', #18684, #4108, #11185, .T. ) ;
#15906 = PRODUCT_RELATED_PRODUCT_CATEGORY ( 'part', '', ( #14221 ) ) ;
#15907 = VECTOR ( 'NONE', #6325, 1000.000000000000000 ) ;
#15908 = ORIENTED_EDGE ( 'NONE', *, *, #750, .T. ) ;
#15909 = VECTOR ( 'NONE', #18640, 1000.000000000000000 ) ;
#15910 = LINE ( 'NONE', #18682, #791 ) ;
#15911 = DIRECTION ( 'NONE',  ( 0.000000000000000000, 0.000000000000000000, -1.000000000000000000 ) ) ;
#15912 = DIRECTION ( 'NONE',  ( 6.982962677686266711E-15, 0.000000000000000000, 1.000000000000000000 ) ) ;
#15913 = CARTESIAN_POINT ( 'NONE',  ( -14.94814811854910275, 76.83212392882506947, 132.4711112102474146 ) ) ;
#15914 = LINE ( 'NONE', #17459, #5521 ) ;
#15915 = EDGE_CURVE ( 'NONE', #13875, #4038, #209, .T. ) ;
#15916 = DIRECTION ( 'NONE',  ( -0.000000000000000000, -0.000000000000000000, 1.000000000000000000 ) ) ;
#15917 = LINE ( 'NONE', #6810, #10117 ) ;
#15918 = CARTESIAN_POINT ( 'NONE',  ( 105.6220017318342599, -121.8343408522480757, 39.87492654200375597 ) ) ;
#15919 = DIRECTION ( 'NONE',  ( -6.982962677686266711E-15, 0.000000000000000000, -1.000000000000000000 ) ) ;
#15920 = EDGE_LOOP ( 'NONE', ( #14033, #12113, #694, #19374 ) ) ;
#15921 = CARTESIAN_POINT ( 'NONE',  ( 134.3599121685105331, -75.61163470463371539, 34.89991303621640384 ) ) ;
#15922 = DIRECTION ( 'NONE',  ( -6.982962677686266711E-15, 0.000000000000000000, -1.000000000000000000 ) ) ;
#15923 = VERTEX_POINT ( 'NONE', #6466 ) ;
#15925 = ORIENTED_EDGE ( 'NONE', *, *, #11507, .F. ) ;
#15924 = AXIS2_PLACEMENT_3D ( 'NONE', #19221, #19319, #16147 ) ;
#15926 = ORIENTED_EDGE ( 'NONE', *, *, #17307, .F. ) ;
#15927 = ADVANCED_FACE ( 'NONE', ( #19343, #2165, #8389, #17814, #3784, #15768 ), #419, .T. ) ;
#15928 = ORIENTED_EDGE ( 'NONE', *, *, #12205, .T. ) ;
#15929 = LINE ( 'NONE', #15520, #10877 ) ;
#15930 = ORIENTED_EDGE ( 'NONE', *, *, #6197, .T. ) ;
#15931 = DIRECTION ( 'NONE',  ( -0.000000000000000000, -0.000000000000000000, 1.000000000000000000 ) ) ;
#15932 = ADVANCED_FACE ( 'NONE', ( #18199 ), #1105, .F. ) ;
#15933 = CARTESIAN_POINT ( 'NONE',  ( -98.17567701213376097, -133.0624052623789453, 33.63793053978134395 ) ) ;
#15934 = FILL_AREA_STYLE_COLOUR ( '', #2093 ) ;
#15935 = DIRECTION ( 'NONE',  ( 0.000000000000000000, 0.000000000000000000, -1.000000000000000000 ) ) ;
#15936 = ORIENTED_EDGE ( 'NONE', *, *, #11927, .F. ) ;
#15937 = CARTESIAN_POINT ( 'NONE',  ( 126.0117988550009898, -81.37275256441674287, -9.384899655049048661 ) ) ;
#15938 = CARTESIAN_POINT ( 'NONE',  ( 31.77187437101505196, 51.77076963420834232, 293.5832628385307999 ) ) ;
#15939 = ORIENTED_EDGE ( 'NONE', *, *, #17969, .T. ) ;
#15940 = AXIS2_PLACEMENT_3D ( 'NONE', #8059, #11025, #3265 ) ;
#15941 = VECTOR ( 'NONE', #12935, 1000.000000000000000 ) ;
#15942 = LINE ( 'NONE', #8157, #10653 ) ;
#15943 = PLANE ( 'NONE',  #8465 ) ;
#15944 = CARTESIAN_POINT ( 'NONE',  ( -75.71267875615008336, -86.11264925328200093, 39.88498244535598047 ) ) ;
#15945 = CARTESIAN_POINT ( 'NONE',  ( 45.46712722958809394, -40.27908801170008246, 283.5832628385307999 ) ) ;
#15946 = PLANE ( 'NONE',  #4833 ) ;
#15947 = DIRECTION ( 'NONE',  ( -0.000000000000000000, -0.000000000000000000, -1.000000000000000000 ) ) ;
#15948 = CARTESIAN_POINT ( 'NONE',  ( 82.03125000000002842, -125.5821405433014064, 31.45421909404266003 ) ) ;
#15949 = VERTEX_POINT ( 'NONE', #2265 ) ;
#15950 = DIRECTION ( 'NONE',  ( -0.6427876096865456912, 0.7660444431189726844, 0.000000000000000000 ) ) ;
#15951 = EDGE_LOOP ( 'NONE', ( #9281, #3426, #3442, #6140 ) ) ;
#15952 = VECTOR ( 'NONE', #17143, 1000.000000000000227 ) ;
#15953 = ORIENTED_EDGE ( 'NONE', *, *, #11967, .T. ) ;
#15954 = CARTESIAN_POINT ( 'NONE',  ( 7.350000000000000533, 5.196152422706624030, -9.000000000000001776 ) ) ;
#15955 = VECTOR ( 'NONE', #7230, 1000.000000000000000 ) ;
#15956 = ORIENTED_EDGE ( 'NONE', *, *, #1883, .F. ) ;
#15957 = FACE_OUTER_BOUND ( 'NONE', #13355, .T. ) ;
#15958 = DIRECTION ( 'NONE',  ( -0.000000000000000000, -0.000000000000000000, 1.000000000000000000 ) ) ;
#15959 = VERTEX_POINT ( 'NONE', #715 ) ;
#15960 = SURFACE_STYLE_FILL_AREA ( #2051 ) ;
#15961 = DIRECTION ( 'NONE',  ( -0.000000000000000000, -0.000000000000000000, 1.000000000000000000 ) ) ;
#15962 = DIRECTION ( 'NONE',  ( 0.000000000000000000, 0.000000000000000000, -1.000000000000000000 ) ) ;
#15963 = DIRECTION ( 'NONE',  ( -0.000000000000000000, -0.000000000000000000, 1.000000000000000000 ) ) ;
#15964 = VECTOR ( 'NONE', #14322, 1000.000000000000000 ) ;
#15965 = VECTOR ( 'NONE', #2800, 1000.000000000000000 ) ;
#15966 = CIRCLE ( 'NONE', #15647, 62.91752772691707207 ) ;
#15967 = FACE_OUTER_BOUND ( 'NONE', #9535, .T. ) ;
#15968 = FACE_OUTER_BOUND ( 'NONE', #13032, .T. ) ;
#15969 = VECTOR ( 'NONE', #7065, 1000.000000000000114 ) ;
#15970 = EDGE_LOOP ( 'NONE', ( #973, #10902, #19410, #11186 ) ) ;
#15971 = CARTESIAN_POINT ( 'NONE',  ( -59.42266395395758138, 50.93469132750324491, 110.7293897666001214 ) ) ;
#15972 = DIRECTION ( 'NONE',  ( -0.000000000000000000, -0.000000000000000000, 1.000000000000000000 ) ) ;
#15973 = CARTESIAN_POINT ( 'NONE',  ( -3.123743752084084058, 4.811834253409051243, 293.5832628385307999 ) ) ;
#15974 = DIRECTION ( 'NONE',  ( 6.982962677686266711E-15, -0.000000000000000000, 1.000000000000000000 ) ) ;
#15975 = VERTEX_POINT ( 'NONE', #2658 ) ;
#15976 = CARTESIAN_POINT ( 'NONE',  ( -109.5721339228237667, 31.03941509555038181, 14.88498244535621851 ) ) ;
#15977 = CARTESIAN_POINT ( 'NONE',  ( -105.5833827013284179, 106.5503530635426728, 44.76066109344641575 ) ) ;
#15978 = EDGE_LOOP ( 'NONE', ( #7640, #11565, #4089, #7541 ) ) ;
#15979 = EDGE_LOOP ( 'NONE', ( #6089, #16006, #2224, #19084 ) ) ;
#15980 = ORIENTED_EDGE ( 'NONE', *, *, #9861, .T. ) ;
#15981 = CONTEXT_DEPENDENT_SHAPE_REPRESENTATION ( #15074, #4574 ) ;
#15982 = CIRCLE ( 'NONE', #7156, 62.91752772691707207 ) ;
#15983 = EDGE_LOOP ( 'NONE', ( #19325, #4986, #8835 ) ) ;
#15984 = AXIS2_PLACEMENT_3D ( 'NONE', #8945, #5585, #5690 ) ;
#15985 = ADVANCED_FACE ( 'NONE', ( #7062 ), #812, .F. ) ;
#15986 = VECTOR ( 'NONE', #8750, 1000.000000000000000 ) ;
#15987 = CARTESIAN_POINT ( 'NONE',  ( -5.590028426173815568, -1.289614712049183209, 293.5832628385307999 ) ) ;
#15988 = EDGE_LOOP ( 'NONE', ( #5043, #19811, #5306, #7351 ) ) ;
#15989 = CARTESIAN_POINT ( 'NONE',  ( -44.07268132743698175, -38.78191089773056177, 110.7293897666001214 ) ) ;
#15990 = FACE_OUTER_BOUND ( 'NONE', #11951, .T. ) ;
#15991 = ADVANCED_FACE ( 'NONE', ( #18305 ), #3978, .F. ) ;
#15992 = VECTOR ( 'NONE', #17937, 1000.000000000000000 ) ;
#15993 = CARTESIAN_POINT ( 'NONE',  ( -131.0756278511784387, 49.33196612817722126, 32.98962906955656393 ) ) ;
#15994 = FACE_OUTER_BOUND ( 'NONE', #15951, .T. ) ;
#15995 = ADVANCED_FACE ( 'NONE', ( #3888 ), #2356, .T. ) ;
#15996 = CARTESIAN_POINT ( 'NONE',  ( -149.8786630148831307, 6.156332247747114295, 1.822476016178801173 ) ) ;
#15997 = EDGE_CURVE ( 'NONE', #7864, #15086, #1056, .T. ) ;
#15998 = LINE ( 'NONE', #18976, #10171 ) ;
#15999 = DIRECTION ( 'NONE',  ( -0.000000000000000000, -0.000000000000000000, 1.000000000000000000 ) ) ;
#16000 = AXIS2_PLACEMENT_3D ( 'NONE', #18755, #14135, #7796 ) ;
#16001 = PLANE ( 'NONE',  #16510 ) ;
#16002 = AXIS2_PLACEMENT_3D ( 'NONE', #13958, #18785, #2823 ) ;
#16003 = ORIENTED_EDGE ( 'NONE', *, *, #10969, .F. ) ;
#16004 = EDGE_CURVE ( 'NONE', #14853, #11236, #5525, .T. ) ;
#16005 = FACE_OUTER_BOUND ( 'NONE', #505, .T. ) ;
#16006 = ORIENTED_EDGE ( 'NONE', *, *, #2607, .T. ) ;
#16007 = ORIENTED_EDGE ( 'NONE', *, *, #11670, .F. ) ;
#16008 = ADVANCED_FACE ( 'NONE', ( #19727 ), #8880, .F. ) ;
#16009 = ORIENTED_EDGE ( 'NONE', *, *, #6362, .T. ) ;
#16010 = AXIS2_PLACEMENT_3D ( 'NONE', #14520, #17895, #19037 ) ;
#16011 = LINE ( 'NONE', #13025, #16131 ) ;
#16012 = AXIS2_PLACEMENT_3D ( 'NONE', #19671, #16708, #16417 ) ;
#16013 = LINE ( 'NONE', #17952, #2754 ) ;
#16014 = FACE_OUTER_BOUND ( 'NONE', #14300, .T. ) ;
#16015 = CIRCLE ( 'NONE', #5001, 110.0000000000000142 ) ;
#16016 = CARTESIAN_POINT ( 'NONE',  ( -136.2050403295488081, -31.16119972761966750, -14.14170230107002268 ) ) ;
#16017 = VERTEX_POINT ( 'NONE', #13379 ) ;
#16018 = DIRECTION ( 'NONE',  ( -0.000000000000000000, -0.000000000000000000, -1.000000000000000000 ) ) ;
#16019 = DIRECTION ( 'NONE',  ( -0.000000000000000000, -0.000000000000000000, 1.000000000000000000 ) ) ;
#16020 = LINE ( 'NONE', #1898, #20236 ) ;
#16021 = ADVANCED_FACE ( 'NONE', ( #15124 ), #6959, .T. ) ;
#16022 = CARTESIAN_POINT ( 'NONE',  ( 103.4088548222097046, -125.4447869035479073, 39.12902662653470287 ) ) ;
#16023 = CARTESIAN_POINT ( 'NONE',  ( 48.17797692984161984, 36.99387960884179449, 293.5832628385307999 ) ) ;
#16024 = ADVANCED_FACE ( 'NONE', ( #13579 ), #16477, .F. ) ;
#16025 = AXIS2_PLACEMENT_3D ( 'NONE', #5011, #17286, #14098 ) ;
#16026 = VECTOR ( 'NONE', #5447, 1000.000000000000000 ) ;
#16027 = AXIS2_PLACEMENT_3D ( 'NONE', #13524, #19773, #5769 ) ;
#16028 = LINE ( 'NONE', #2010, #9681 ) ;
#16029 = ORIENTED_EDGE ( 'NONE', *, *, #3159, .F. ) ;
#16030 = ORIENTED_EDGE ( 'NONE', *, *, #10607, .F. ) ;
#16031 = VERTEX_POINT ( 'NONE', #5823 ) ;
#16032 = ORIENTED_EDGE ( 'NONE', *, *, #9238, .F. ) ;
#16033 = ADVANCED_FACE ( 'NONE', ( #4078 ), #8686, .F. ) ;
#16034 = ORIENTED_EDGE ( 'NONE', *, *, #2402, .T. ) ;
#16035 = DIRECTION ( 'NONE',  ( -1.000000000000000000, 0.000000000000000000, 0.000000000000000000 ) ) ;
#16036 = DIRECTION ( 'NONE',  ( 6.982962677686266711E-15, -0.000000000000000000, 1.000000000000000000 ) ) ;
#16037 = PLANE ( 'NONE',  #7634 ) ;
#16038 = DIRECTION ( 'NONE',  ( -0.9848077530122062440, -0.1736481776669404620, 0.000000000000000000 ) ) ;
#16039 = EDGE_LOOP ( 'NONE', ( #19105, #19662 ) ) ;
#16040 = CIRCLE ( 'NONE', #3625, 62.91752772691707207 ) ;
#16041 = DIRECTION ( 'NONE',  ( 0.000000000000000000, 0.000000000000000000, -1.000000000000000000 ) ) ;
#16042 = CARTESIAN_POINT ( 'NONE',  ( -57.65577537092151772, 11.00103590902930328, 248.9926560891072143 ) ) ;
#16043 = VERTEX_POINT ( 'NONE', #18103 ) ;
#16044 = FACE_OUTER_BOUND ( 'NONE', #8670, .T. ) ;
#16045 = CARTESIAN_POINT ( 'NONE',  ( 0.000000000000000000, 0.000000000000000000, 0.000000000000000000 ) ) ;
#16046 = ADVANCED_FACE ( 'NONE', ( #12044 ), #19632, .F. ) ;
#16047 = FACE_OUTER_BOUND ( 'NONE', #17602, .T. ) ;
#16048 = EDGE_CURVE ( 'NONE', #2266, #18696, #7925, .T. ) ;
#16049 = DIRECTION ( 'NONE',  ( -6.982962677686266711E-15, 0.000000000000000000, -1.000000000000000000 ) ) ;
#16050 = CARTESIAN_POINT ( 'NONE',  ( 0.000000000000000000, 0.000000000000000000, -9.999999999999987566 ) ) ;
#16051 = CARTESIAN_POINT ( 'NONE',  ( -67.08601213326568313, -40.32479851956793482, 110.9660488491356887 ) ) ;
#16052 = CARTESIAN_POINT ( 'NONE',  ( -75.01458320008653402, 118.2066678791461953, 6.325805891068640108 ) ) ;
#16053 = ADVANCED_FACE ( 'NONE', ( #4180 ), #10413, .F. ) ;
#16054 = VERTEX_POINT ( 'NONE', #6035 ) ;
#16055 = VECTOR ( 'NONE', #9597, 1000.000000000000000 ) ;
#16056 = FACE_OUTER_BOUND ( 'NONE', #10320, .T. ) ;
#16057 = EDGE_CURVE ( 'NONE', #9227, #17450, #9399, .T. ) ;
#16058 = ORIENTED_EDGE ( 'NONE', *, *, #438, .F. ) ;
#16059 = VECTOR ( 'NONE', #15172, 1000.000000000000000 ) ;
#16060 = ORIENTED_EDGE ( 'NONE', *, *, #8886, .F. ) ;
#16061 = FACE_OUTER_BOUND ( 'NONE', #15463, .T. ) ;
#16062 = ORIENTED_EDGE ( 'NONE', *, *, #15277, .F. ) ;
#16063 = AXIS2_PLACEMENT_3D ( 'NONE', #1263, #10872, #10561 ) ;
#16064 = DIRECTION ( 'NONE',  ( 0.000000000000000000, 1.000000000000000000, 0.000000000000000000 ) ) ;
#16065 = FACE_OUTER_BOUND ( 'NONE', #7358, .T. ) ;
#16066 = VERTEX_POINT ( 'NONE', #17185 ) ;
#16067 = PRESENTATION_STYLE_ASSIGNMENT (( #12782 ) ) ;
#16068 = LINE ( 'NONE', #14817, #6053 ) ;
#16069 = CARTESIAN_POINT ( 'NONE',  ( 41.02350267428969488, 44.79940644582669051, 293.5832628385307999 ) ) ;
#16070 = DIRECTION ( 'NONE',  ( -0.000000000000000000, -0.000000000000000000, -1.000000000000000000 ) ) ;
#16071 = DIRECTION ( 'NONE',  ( -1.000000000000000000, 0.000000000000000000, 0.000000000000000000 ) ) ;
#16072 = CARTESIAN_POINT ( 'NONE',  ( 50.37374754117451658, -141.2886604036502831, 49.99999999999999289 ) ) ;
#16073 = ORIENTED_EDGE ( 'NONE', *, *, #13903, .T. ) ;
#16074 = DIRECTION ( 'NONE',  ( 0.000000000000000000, 0.000000000000000000, 1.000000000000000000 ) ) ;
#16075 = CARTESIAN_POINT ( 'NONE',  ( 7.350000000000000533, -5.196152422706636465, -8.999999999999998224 ) ) ;
#16076 = DIRECTION ( 'NONE',  ( 0.000000000000000000, 0.000000000000000000, 1.000000000000000000 ) ) ;
#16077 = DIRECTION ( 'NONE',  ( 0.000000000000000000, 0.000000000000000000, -1.000000000000000000 ) ) ;
#16078 = ORIENTED_EDGE ( 'NONE', *, *, #7854, .T. ) ;
#16079 = CARTESIAN_POINT ( 'NONE',  ( -30.05702882063063086, -50.41613078340792242, 248.9926560891072143 ) ) ;
#16080 = FACE_OUTER_BOUND ( 'NONE', #12240, .T. ) ;
#16081 = EDGE_LOOP ( 'NONE', ( #11895, #5477, #9876, #19153 ) ) ;
#16082 = ORIENTED_EDGE ( 'NONE', *, *, #19496, .F. ) ;
#16083 = ORIENTED_EDGE ( 'NONE', *, *, #5759, .T. ) ;
#16084 = CONTEXT_DEPENDENT_SHAPE_REPRESENTATION ( #7109, #14564 ) ;
#16085 = ORIENTED_EDGE ( 'NONE', *, *, #13127, .T. ) ;
#16086 = DIRECTION ( 'NONE',  ( 0.3088643371590125142, -0.9511061040868803440, 0.000000000000000000 ) ) ;
#16087 = CARTESIAN_POINT ( 'NONE',  ( -149.2033348278766027, 15.60004678097522657, 13.02734773726837147 ) ) ;
#16088 = VERTEX_POINT ( 'NONE', #13791 ) ;
#16089 = VECTOR ( 'NONE', #5161, 1000.000000000000114 ) ;
#16090 = CARTESIAN_POINT ( 'NONE',  ( -117.2142335457655520, -12.13581325405623268, 14.88498244535627002 ) ) ;
#16091 = DIRECTION ( 'NONE',  ( -0.9394263059140720573, -0.3427509529624101492, 0.000000000000000000 ) ) ;
#16092 = CARTESIAN_POINT ( 'NONE',  ( -98.30983243222962642, -132.8827373471657722, 6.041609267868833122 ) ) ;
#16093 = ORIENTED_EDGE ( 'NONE', *, *, #3781, .F. ) ;
#16094 = PLANE ( 'NONE',  #14060 ) ;
#16095 = DIRECTION ( 'NONE',  ( 0.4999999999999919509, 0.8660254037844432595, 0.000000000000000000 ) ) ;
#16096 = DIRECTION ( 'NONE',  ( -0.4974449862757516216, 6.091944101944981818E-17, 0.8674955248467378643 ) ) ;
#16097 = DIRECTION ( 'NONE',  ( -0.000000000000000000, -0.000000000000000000, 1.000000000000000000 ) ) ;
#16098 = DIRECTION ( 'NONE',  ( 1.000000000000000000, 0.000000000000000000, 0.000000000000000000 ) ) ;
#16099 = CARTESIAN_POINT ( 'NONE',  ( -130.9868171408399746, -91.88282611735537841, 40.00000000000000000 ) ) ;
#16100 = ADVANCED_FACE ( 'NONE', ( #7654 ), #6241, .T. ) ;
#16101 = EDGE_LOOP ( 'NONE', ( #19453, #14241, #9729, #2544 ) ) ;
#16102 = CARTESIAN_POINT ( 'NONE',  ( -138.1593264817448414, 18.92187976101237368, -15.79357949266177386 ) ) ;
#16103 = AXIS2_PLACEMENT_3D ( 'NONE', #15278, #17132, #6086 ) ;
#16104 = EDGE_LOOP ( 'NONE', ( #15745, #9960 ) ) ;
#16105 = AXIS2_PLACEMENT_3D ( 'NONE', #11747, #7165, #5429 ) ;
#16106 = ORIENTED_EDGE ( 'NONE', *, *, #899, .T. ) ;
#16107 = EDGE_CURVE ( 'NONE', #15546, #12565, #15105, .T. ) ;
#16108 = ORIENTED_EDGE ( 'NONE', *, *, #16534, .T. ) ;
#16109 = EDGE_CURVE ( 'NONE', #12588, #3447, #4593, .T. ) ;
#16110 = DIRECTION ( 'NONE',  ( 0.000000000000000000, 0.000000000000000000, 1.000000000000000000 ) ) ;
#16111 = CIRCLE ( 'NONE', #7282, 62.91752772691707207 ) ;
#16112 = DIRECTION ( 'NONE',  ( 0.9848077530122097967, -0.1736481776669207000, 0.000000000000000000 ) ) ;
#16113 = VECTOR ( 'NONE', #10025, 1000.000000000000000 ) ;
#16114 = DIRECTION ( 'NONE',  ( 0.000000000000000000, 0.000000000000000000, 1.000000000000000000 ) ) ;
#16115 = CARTESIAN_POINT ( 'NONE',  ( -71.18887634719365565, -147.8252249328922687, 60.00000000000000000 ) ) ;
#16116 = CARTESIAN_POINT ( 'NONE',  ( -9.564549117045515914, -62.18629025319810211, 293.5832628385307999 ) ) ;
#16117 = PLANE ( 'NONE',  #17642 ) ;
#16118 = AXIS2_PLACEMENT_3D ( 'NONE', #3372, #11344, #16458 ) ;
#16119 = CARTESIAN_POINT ( 'NONE',  ( 14.39940464655707331, 76.92888220842492331, 248.9926560891072143 ) ) ;
#16120 = DIRECTION ( 'NONE',  ( -0.000000000000000000, -1.000000000000000000, -0.000000000000000000 ) ) ;
#16121 = EDGE_CURVE ( 'NONE', #6626, #15899, #1318, .T. ) ;
#16122 = VERTEX_POINT ( 'NONE', #90 ) ;
#16123 = VERTEX_POINT ( 'NONE', #2857 ) ;
#16124 = AXIS2_PLACEMENT_3D ( 'NONE', #815, #3787, #10033 ) ;
#16125 = ORIENTED_EDGE ( 'NONE', *, *, #14892, .F. ) ;
#16126 = ORIENTED_EDGE ( 'NONE', *, *, #5153, .F. ) ;
#16127 = CARTESIAN_POINT ( 'NONE',  ( -0.8220851292435327196, -78.26059000578311498, 112.7772637782949943 ) ) ;
#16128 = EDGE_CURVE ( 'NONE', #13973, #6346, #9561, .T. ) ;
#16129 = ORIENTED_EDGE ( 'NONE', *, *, #15079, .T. ) ;
#16130 = EDGE_CURVE ( 'NONE', #6087, #5083, #7551, .T. ) ;
#16131 = VECTOR ( 'NONE', #2299, 1000.000000000000000 ) ;
#16132 = EDGE_CURVE ( 'NONE', #4680, #5679, #6899, .T. ) ;
#16133 = DIRECTION ( 'NONE',  ( 0.7660444431189771253, 0.6427876096865404731, 0.000000000000000000 ) ) ;
#16134 = DIRECTION ( 'NONE',  ( -0.000000000000000000, -0.000000000000000000, 1.000000000000000000 ) ) ;
#16135 = PRESENTATION_LAYER_ASSIGNMENT (  '', '', ( #18100 ) ) ;
#16136 = DIRECTION ( 'NONE',  ( 0.4338837391175549563, 0.9009688679024205893, 0.000000000000000000 ) ) ;
#16137 = ORIENTED_EDGE ( 'NONE', *, *, #8520, .T. ) ;
#16138 = CARTESIAN_POINT ( 'NONE',  ( 27.90514497005375461, -110.4119590718113244, 14.88498244535525750 ) ) ;
#16139 = DIRECTION ( 'NONE',  ( -1.613511099790691498E-16, 1.000000000000000000, 0.000000000000000000 ) ) ;
#16140 = ORIENTED_EDGE ( 'NONE', *, *, #19033, .F. ) ;
#16141 = CARTESIAN_POINT ( 'NONE',  ( 128.2779226595531270, 102.2982297021113141, 39.99999999999999289 ) ) ;
#16142 = DIRECTION ( 'NONE',  ( -0.000000000000000000, -0.000000000000000000, 1.000000000000000000 ) ) ;
#16143 = DIRECTION ( 'NONE',  ( -1.000000000000000000, 0.000000000000000000, 0.000000000000000000 ) ) ;
#16144 = B_SPLINE_CURVE_WITH_KNOTS ( 'NONE', 3,
 ( #7487, #12187, #19567, #14958, #5560, #16704, #13725, #15259, #2689, #13515, #18137, #11781, #19866, #18043, #4217, #18341, #8821, #15061, #19766, #10446, #8918, #9124, #4315, #15162, #16604, #1144, #18235, #16511 ),
 .UNSPECIFIED., .F., .F.,
 ( 4, 2, 2, 2, 2, 2, 2, 2, 2, 2, 2, 2, 2, 4 ),
 ( 0.000000000000000000, 0.001466376146900906291, 0.002199564220351354991, 0.002932752293801805642, 0.004399128440702712584, 0.005865504587603619958, 0.007331880734504528201, 0.008798256881405435575, 0.01026463302830634382, 0.01173100917520725033, 0.01466376146900906334, 0.01759651376281088156, 0.02052926605661269457, 0.02346201835041451106 ),
 .UNSPECIFIED. ) ;
#16145 = DIRECTION ( 'NONE',  ( 1.000000000000000000, 0.000000000000000000, 0.000000000000000000 ) ) ;
#16146 = ADVANCED_FACE ( 'NONE', ( #3267 ), #2037, .F. ) ;
#16147 = DIRECTION ( 'NONE',  ( -0.7660444431189770143, 0.6427876096865404731, 5.346191897317644012E-15 ) ) ;
#16148 = AXIS2_PLACEMENT_3D ( 'NONE', #8507, #3799, #11474 ) ;
#16149 = LINE ( 'NONE', #16347, #1719 ) ;
#16150 = CARTESIAN_POINT ( 'NONE',  ( 95.41207185104578059, -115.7515782192335081, 49.20090002619129166 ) ) ;
#16151 = ORIENTED_EDGE ( 'NONE', *, *, #3412, .F. ) ;
#16152 = B_SPLINE_CURVE_WITH_KNOTS ( 'NONE', 3,
 ( #8223, #12927, #6804, #5176, #19185, #13027, #2300, #17844, #19570, #13213, #2098, #5561, #11494, #14764, #11783, #17745, #3821, #16212, #14670, #751, #657, #6902, #13115, #6996 ),
 .UNSPECIFIED., .F., .F.,
 ( 4, 2, 2, 2, 2, 2, 2, 2, 2, 2, 2, 4 ),
 ( 0.000000000000000000, 0.002185557465519409343, 0.004371114931038821289, 0.008742229862077633903, 0.01311334479311644652, 0.01529890225863585543, 0.01748445972415526087, 0.02185557465519410644, 0.02404113212071354658, 0.02622668958623298671, 0.03059780451727186351, 0.03496891944831072296 ),
 .UNSPECIFIED. ) ;
#16153 = CARTESIAN_POINT ( 'NONE',  ( -110.0000000000000142, 1.347111479062088839E-14, -9.999999999999994671 ) ) ;
#16154 = VECTOR ( 'NONE', #3653, 1000.000000000000227 ) ;
#16155 = VERTEX_POINT ( 'NONE', #8263 ) ;
#16156 = ORIENTED_EDGE ( 'NONE', *, *, #8781, .F. ) ;
#16157 = DIRECTION ( 'NONE',  ( 0.000000000000000000, 1.000000000000000000, 0.000000000000000000 ) ) ;
#16158 = EDGE_LOOP ( 'NONE', ( #13693, #12129, #1299, #13858 ) ) ;
#16159 = EDGE_CURVE ( 'NONE', #12285, #18229, #4690, .T. ) ;
#16160 = EDGE_CURVE ( 'NONE', #11536, #8815, #1935, .T. ) ;
#16161 = ADVANCED_FACE ( 'NONE', ( #15848 ), #11027, .T. ) ;
#16162 = ADVANCED_FACE ( 'NONE', ( #292 ), #6547, .T. ) ;
#16163 = EDGE_CURVE ( 'NONE', #274, #18902, #2192, .T. ) ;
#16164 = LINE ( 'NONE', #3676, #4194 ) ;
#16165 = CARTESIAN_POINT ( 'NONE',  ( -82.06839719201970240, -125.5578986320909962, 31.45126808048254219 ) ) ;
#16166 = AXIS2_PLACEMENT_3D ( 'NONE', #16569, #14823, #4073 ) ;
#16167 = SURFACE_SIDE_STYLE ('',( #15960 ) ) ;
#16168 = CARTESIAN_POINT ( 'NONE',  ( -109.9999999999983515, 275.0000000000000000, 92.50000000000004263 ) ) ;
#16169 = DIRECTION ( 'NONE',  ( 0.6692498792541753394, 0.7430374143461900838, 0.000000000000000000 ) ) ;
#16170 = CIRCLE ( 'NONE', #2119, 60.74260934110282051 ) ;
#16171 = DIRECTION ( 'NONE',  ( 1.000000000000000000, 0.000000000000000000, 0.000000000000000000 ) ) ;
#16172 = CARTESIAN_POINT ( 'NONE',  ( 99.30949456653218022, -131.5229532012208722, 4.208660560896509750 ) ) ;
#16173 = CARTESIAN_POINT ( 'NONE',  ( -12.14957802882752524, -59.51724408343569905, 283.5832628385307999 ) ) ;
#16174 = CARTESIAN_POINT ( 'NONE',  ( 2.240720816136073434, -5.281164089014820817, 283.5832628385307999 ) ) ;
#16175 = DIRECTION ( 'NONE',  ( 0.000000000000000000, 0.000000000000000000, 1.000000000000000000 ) ) ;
#16176 = LINE ( 'NONE', #8388, #11113 ) ;
#16177 = AXIS2_PLACEMENT_3D ( 'NONE', #15580, #5057, #131 ) ;
#16178 = DIRECTION ( 'NONE',  ( -0.8830229359480271656, -0.4693298356057563625, 0.000000000000000000 ) ) ;
#16179 = ORIENTED_EDGE ( 'NONE', *, *, #6776, .T. ) ;
#16180 = CARTESIAN_POINT ( 'NONE',  ( -122.8001410695374460, -86.14014948502065749, 49.99999999999999289 ) ) ;
#16181 = DIRECTION ( 'NONE',  ( 1.000000000000000000, 0.000000000000000000, -6.976128451377902853E-15 ) ) ;
#16182 = ORIENTED_EDGE ( 'NONE', *, *, #19259, .T. ) ;
#16183 = CIRCLE ( 'NONE', #9962, 106.4288957539801146 ) ;
#16184 = VERTEX_POINT ( 'NONE', #4055 ) ;
#16185 = SHAPE_REPRESENTATION ( 'Upper Flange', ( #18639 ), #14384 ) ;
#16186 = EDGE_LOOP ( 'NONE', ( #4214, #14274, #2894, #19027 ) ) ;
#16187 = CONTEXT_DEPENDENT_SHAPE_REPRESENTATION ( #8802, #17676 ) ;
#16188 = EDGE_CURVE ( 'NONE', #2555, #2184, #8058, .T. ) ;
#16189 = ORIENTED_EDGE ( 'NONE', *, *, #16491, .F. ) ;
#16190 = CARTESIAN_POINT ( 'NONE',  ( -110.0000000000000284, 101.9803902718557111, 44.99999999999998579 ) ) ;
#16191 = EDGE_LOOP ( 'NONE', ( #13713, #217, #19831, #2938 ) ) ;
#16192 = CIRCLE ( 'NONE', #1814, 127.4413876050234649 ) ;
#16193 = DIRECTION ( 'NONE',  ( 6.982962677686266711E-15, -0.000000000000000000, 1.000000000000000000 ) ) ;
#16194 = LINE ( 'NONE', #14558, #7631 ) ;
#16195 = CARTESIAN_POINT ( 'NONE',  ( -95.42019791134576678, -116.1393900958301231, 7.897240193129543506 ) ) ;
#16196 = EDGE_LOOP ( 'NONE', ( #13448, #17926, #11660, #15228 ) ) ;
#16197 = EDGE_CURVE ( 'NONE', #17104, #2440, #4125, .T. ) ;
#16198 = CARTESIAN_POINT ( 'NONE',  ( -139.6219990602459120, -10.61388033341743942, 23.64454228650399870 ) ) ;
#16199 = PLANE ( 'NONE',  #6908 ) ;
#16200 = DIRECTION ( 'NONE',  ( 1.000000000000000000, 0.000000000000000000, -6.994638739193269649E-15 ) ) ;
#16201 = LINE ( 'NONE', #6983, #9190 ) ;
#16202 = CARTESIAN_POINT ( 'NONE',  ( 51.77076963420847733, -31.77187437101486367, 283.5832628385307999 ) ) ;
#16203 = CARTESIAN_POINT ( 'NONE',  ( -131.2702496982249727, -90.86622748991179321, 40.00000000000000000 ) ) ;
#16204 = VERTEX_POINT ( 'NONE', #2529 ) ;
#16205 = DIRECTION ( 'NONE',  ( 1.000000000000000000, 0.000000000000000000, 0.000000000000000000 ) ) ;
#16206 = PRESENTATION_LAYER_ASSIGNMENT (  '', '', ( #14240 ) ) ;
#16207 = ORIENTED_EDGE ( 'NONE', *, *, #8872, .T. ) ;
#16208 = EDGE_LOOP ( 'NONE', ( #1459, #13257, #17862, #6921 ) ) ;
#16209 = EDGE_LOOP ( 'NONE', ( #14668, #18163, #9251, #579 ) ) ;
#16210 = DIRECTION ( 'NONE',  ( 0.000000000000000000, 0.000000000000000000, 1.000000000000000000 ) ) ;
#16211 = AXIS2_PLACEMENT_3D ( 'NONE', #2206, #16518, #18144 ) ;
#16212 = CARTESIAN_POINT ( 'NONE',  ( -128.2054629363889831, -77.87043913366071024, -8.142599671304674658 ) ) ;
#16213 = DIRECTION ( 'NONE',  ( 0.7881095627315598540, 0.6155349844899715706, 0.000000000000000000 ) ) ;
#16214 = CARTESIAN_POINT ( 'NONE',  ( 0.01885174614965866302, 0.8831628876357845437, -9.000000000000001776 ) ) ;
#16215 = B_SPLINE_CURVE_WITH_KNOTS ( 'NONE', 3,
 ( #2204, #9862, #11496, #14273, #19289, #16214, #9966, #19188 ),
 .UNSPECIFIED., .F., .F.,
 ( 4, 2, 2, 4 ),
 ( 0.02518894967656377937, 0.02782118485464665086, 0.02913730244368808661, 0.03045342003272952236 ),
 .UNSPECIFIED. ) ;
#16216 = ORIENTED_EDGE ( 'NONE', *, *, #14472, .F. ) ;
#16217 = CIRCLE ( 'NONE', #6397, 60.74260934110282051 ) ;
#16218 = DIRECTION ( 'NONE',  ( -0.9993852124581887875, 0.03505990758545545621, 0.000000000000000000 ) ) ;
#16219 = CARTESIAN_POINT ( 'NONE',  ( -63.68887634719365565, -147.8252249328922687, 39.99999999999999289 ) ) ;
#16220 = LINE ( 'NONE', #18146, #3345 ) ;
#16221 = CARTESIAN_POINT ( 'NONE',  ( -11.73417718768092044, -61.81362617575097573, 248.9926560891072143 ) ) ;
#16222 = DIRECTION ( 'NONE',  ( -1.000000000000000000, 0.000000000000000000, 6.982962677686266711E-15 ) ) ;
#16223 = DIRECTION ( 'NONE',  ( 0.000000000000000000, 0.000000000000000000, 1.000000000000000000 ) ) ;
#16224 = ORIENTED_EDGE ( 'NONE', *, *, #6778, .T. ) ;
#16225 = VECTOR ( 'NONE', #18552, 1000.000000000000000 ) ;
#16226 = EDGE_LOOP ( 'NONE', ( #19306, #4888 ) ) ;
#16227 = VERTEX_POINT ( 'NONE', #7134 ) ;
#16228 = VECTOR ( 'NONE', #372, 1000.000000000000000 ) ;
#16229 = ORIENTED_EDGE ( 'NONE', *, *, #3519, .F. ) ;
#16230 = EDGE_LOOP ( 'NONE', ( #17613, #816, #7789, #1974 ) ) ;
#16231 = DIRECTION ( 'NONE',  ( -0.7660444431189726844, -0.6427876096865458022, 0.000000000000000000 ) ) ;
#16232 = AXIS2_PLACEMENT_3D ( 'NONE', #13352, #19321, #5305 ) ;
#16233 = ORIENTED_EDGE ( 'NONE', *, *, #8420, .T. ) ;
#16234 = EDGE_CURVE ( 'NONE', #16184, #9484, #11534, .T. ) ;
#16235 = CARTESIAN_POINT ( 'NONE',  ( -32.62092819947992695, -51.24245927909985454, 293.5832628385307999 ) ) ;
#16236 = ADVANCED_FACE ( 'NONE', ( #15094 ), #11721, .F. ) ;
#16237 = CARTESIAN_POINT ( 'NONE',  ( -110.0000000000000142, 275.0000000000000000, 5.000000000000000888 ) ) ;
#16238 = CARTESIAN_POINT ( 'NONE',  ( 17.24542129382117750, 20.55229278271219329, 14.88498244535533033 ) ) ;
#16239 = EDGE_LOOP ( 'NONE', ( #19512, #4723, #3739, #3404 ) ) ;
#16240 = CARTESIAN_POINT ( 'NONE',  ( 51.77251465595239921, -31.77296517111717478, 283.5832628385307999 ) ) ;
#16241 = DIRECTION ( 'NONE',  ( 0.1736481776669404620, -0.9848077530122062440, 0.000000000000000000 ) ) ;
#16242 = VECTOR ( 'NONE', #3876, 1000.000000000000000 ) ;
#16243 = ORIENTED_EDGE ( 'NONE', *, *, #6270, .T. ) ;
#16244 = CARTESIAN_POINT ( 'NONE',  ( 54.86954475316255042, -20.84572577951183092, 132.4711112102474146 ) ) ;
#16245 = VECTOR ( 'NONE', #12595, 1000.000000000000000 ) ;
#16246 = DIRECTION ( 'NONE',  ( -0.000000000000000000, -0.000000000000000000, 1.000000000000000000 ) ) ;
#16247 = DIRECTION ( 'NONE',  ( 1.000000000000000000, 0.000000000000000000, 0.000000000000000000 ) ) ;
#16248 = CARTESIAN_POINT ( 'NONE',  ( 49.67518383744835120, -60.47951622432767493, 110.7293897666001214 ) ) ;
#16249 = AXIS2_PLACEMENT_3D ( 'NONE', #4616, #17096, #10433 ) ;
#16250 = ADVANCED_FACE ( 'NONE', ( #1076 ), #14999, .F. ) ;
#16251 = EDGE_CURVE ( 'NONE', #2918, #12798, #10662, .T. ) ;
#16252 = CARTESIAN_POINT ( 'NONE',  ( -139.3747594192856525, -22.29693483761631967, -14.06286033225251231 ) ) ;
#16253 = DIRECTION ( 'NONE',  ( 0.4999999999999918954, -0.8660254037844433705, -3.503961184244745387E-15 ) ) ;
#16254 = DIRECTION ( 'NONE',  ( -0.000000000000000000, -0.000000000000000000, 1.000000000000000000 ) ) ;
#16255 = ORIENTED_EDGE ( 'NONE', *, *, #16914, .F. ) ;
#16256 = ADVANCED_FACE ( 'NONE', ( #14704 ), #7231, .F. ) ;
#16257 = CARTESIAN_POINT ( 'NONE',  ( 51.77251465595239921, -31.77296517111717478, 293.5832628385307999 ) ) ;
#16258 = ORIENTED_EDGE ( 'NONE', *, *, #9916, .T. ) ;
#16259 = ORIENTED_EDGE ( 'NONE', *, *, #4652, .F. ) ;
#16260 = DIRECTION ( 'NONE',  ( 1.000000000000000000, 0.000000000000000000, 0.000000000000000000 ) ) ;
#16261 = APPLICATION_CONTEXT ( 'automotive_design' ) ;
#16262 = ORIENTED_EDGE ( 'NONE', *, *, #9559, .F. ) ;
#16263 = ADVANCED_FACE ( 'NONE', ( #3758 ), #10193, .F. ) ;
#16264 = DIRECTION ( 'NONE',  ( 0.000000000000000000, 0.000000000000000000, 1.000000000000000000 ) ) ;
#16265 = VECTOR ( 'NONE', #1005, 1000.000000000000000 ) ;
#16266 = CARTESIAN_POINT ( 'NONE',  ( -86.10242266703171765, -122.8274731153598225, 42.46235246160556898 ) ) ;
#16267 = VECTOR ( 'NONE', #6517, 1000.000000000000114 ) ;
#16268 = DIRECTION ( 'NONE',  ( 1.000000000000000000, 0.000000000000000000, 0.000000000000000000 ) ) ;
#16269 = DIRECTION ( 'NONE',  ( -0.000000000000000000, -0.000000000000000000, 1.000000000000000000 ) ) ;
#16270 = VERTEX_POINT ( 'NONE', #13249 ) ;
#16271 = CARTESIAN_POINT ( 'NONE',  ( 107.5000000000000142, -113.9901311517800053, 0.000000000000000000 ) ) ;
#16272 = CARTESIAN_POINT ( 'NONE',  ( 141.8714406926368099, -48.70825716237082759, 60.00000000000000000 ) ) ;
#16273 = DIRECTION ( 'NONE',  ( 0.000000000000000000, 0.000000000000000000, -1.000000000000000000 ) ) ;
#16274 = DIRECTION ( 'NONE',  ( 0.000000000000000000, 0.000000000000000000, 1.000000000000000000 ) ) ;
#16275 = DIRECTION ( 'NONE',  ( -0.000000000000000000, -0.000000000000000000, -1.000000000000000000 ) ) ;
#16276 = FACE_OUTER_BOUND ( 'NONE', #19943, .T. ) ;
#16277 = EDGE_CURVE ( 'NONE', #2315, #10541, #10000, .T. ) ;
#16278 = DIRECTION ( 'NONE',  ( 0.000000000000000000, 0.000000000000000000, -1.000000000000000000 ) ) ;
#16279 = DIRECTION ( 'NONE',  ( 0.8660254037844397068, -0.4999999999999978906, 0.000000000000000000 ) ) ;
#16280 = VECTOR ( 'NONE', #17353, 1000.000000000000000 ) ;
#16281 = EDGE_CURVE ( 'NONE', #2426, #17841, #14269, .T. ) ;
#16282 = ORIENTED_EDGE ( 'NONE', *, *, #16874, .T. ) ;
#16283 = EDGE_CURVE ( 'NONE', #16530, #17276, #17215, .T. ) ;
#16284 = VECTOR ( 'NONE', #11771, 1000.000000000000000 ) ;
#16285 = PLANE ( 'NONE',  #19230 ) ;
#16286 = CARTESIAN_POINT ( 'NONE',  ( -176.7850001792984926, -190.0000000000000284, 40.00000000000000000 ) ) ;
#16287 = ORIENTED_EDGE ( 'NONE', *, *, #1860, .F. ) ;
#16288 = ORIENTED_EDGE ( 'NONE', *, *, #18426, .F. ) ;
#16289 = EDGE_LOOP ( 'NONE', ( #7862, #15928, #8757, #5191 ) ) ;
#16290 = ADVANCED_BREP_SHAPE_REPRESENTATION ( '', ( #8201, #18639 ), #8174 ) ;
#16291 = ORIENTED_EDGE ( 'NONE', *, *, #18793, .T. ) ;
#16292 = EDGE_CURVE ( 'NONE', #7170, #17700, #3859, .T. ) ;
#16293 = CARTESIAN_POINT ( 'NONE',  ( 57.92709869106709419, 18.28567271940532990, 293.5832628385307999 ) ) ;
#16294 = EDGE_LOOP ( 'NONE', ( #861, #6567, #1188, #8876 ) ) ;
#16295 = CARTESIAN_POINT ( 'NONE',  ( 0.000000000000000000, 0.000000000000000000, 293.5832628385307999 ) ) ;
#16296 = CARTESIAN_POINT ( 'NONE',  ( -101.9588377999664317, -127.6928792353688209, 1.652472148576846545 ) ) ;
#16297 = VERTEX_POINT ( 'NONE', #19606 ) ;
#16298 = CIRCLE ( 'NONE', #17912, 127.4413876050234649 ) ;
#16299 = CARTESIAN_POINT ( 'NONE',  ( -83.45731665390675857, -124.6394201399246384, 2.317304836764386700 ) ) ;
#16300 = DIRECTION ( 'NONE',  ( -0.000000000000000000, -0.000000000000000000, -1.000000000000000000 ) ) ;
#16301 = DIRECTION ( 'NONE',  ( -0.000000000000000000, -0.000000000000000000, 1.000000000000000000 ) ) ;
#16302 = LINE ( 'NONE', #8516, #16423 ) ;
#16303 = ADVANCED_FACE ( 'NONE', ( #5594 ), #10291, .T. ) ;
#16304 = ADVANCED_FACE ( 'NONE', ( #11629 ), #8562, .F. ) ;
#16305 =( NAMED_UNIT ( * ) PLANE_ANGLE_UNIT ( ) SI_UNIT ( $, .RADIAN. ) );
#16306 = CARTESIAN_POINT ( 'NONE',  ( 1.379293853801755176, -62.90240729679781850, 248.9926560891072143 ) ) ;
#16307 = DIRECTION ( 'NONE',  ( 0.6155349844899715706, -0.7881095627315598540, 0.000000000000000000 ) ) ;
#16308 = ORIENTED_EDGE ( 'NONE', *, *, #4772, .T. ) ;
#16309 = CARTESIAN_POINT ( 'NONE',  ( 15.91767397667354800, 164.0736214083062805, 39.99999999999999289 ) ) ;
#16310 = FACE_OUTER_BOUND ( 'NONE', #4206, .T. ) ;
#16311 = CIRCLE ( 'NONE', #3878, 7.500000000000001776 ) ;
#16312 = VECTOR ( 'NONE', #9405, 1000.000000000000000 ) ;
#16313 = EDGE_CURVE ( 'NONE', #9831, #18511, #2334, .T. ) ;
#16314 = CIRCLE ( 'NONE', #1268, 60.74260934110282051 ) ;
#16315 = VERTEX_POINT ( 'NONE', #5800 ) ;
#16316 = FACE_OUTER_BOUND ( 'NONE', #6890, .T. ) ;
#16317 = CARTESIAN_POINT ( 'NONE',  ( -163.5019688434124419, -20.99123081650240863, 49.99999999999999289 ) ) ;
#16318 = PLANE ( 'NONE',  #13665 ) ;
#16319 = CARTESIAN_POINT ( 'NONE',  ( -67.36461649554505016, 39.84224160888970800, 132.4711112102474146 ) ) ;
#16320 = VECTOR ( 'NONE', #5487, 1000.000000000000000 ) ;
#16321 = CARTESIAN_POINT ( 'NONE',  ( -60.47951622432784546, -49.67518383744813804, 248.9926560891072143 ) ) ;
#16322 = CARTESIAN_POINT ( 'NONE',  ( -123.8648416762430884, -84.61253400034597405, -0.6186463947281112263 ) ) ;
#16323 = CARTESIAN_POINT ( 'NONE',  ( 134.7747342791600715, -65.84665809079267262, 5.198213465029171587 ) ) ;
#16324 = CARTESIAN_POINT ( 'NONE',  ( 71.18887634719571622, -147.8252249328912740, 60.00000000000000000 ) ) ;
#16325 = DIRECTION ( 'NONE',  ( -0.8660254037844345998, -0.5000000000000069944, 0.000000000000000000 ) ) ;
#16326 = ORIENTED_EDGE ( 'NONE', *, *, #7039, .T. ) ;
#16327 = VERTEX_POINT ( 'NONE', #13765 ) ;
#16328 = ORIENTED_EDGE ( 'NONE', *, *, #9670, .F. ) ;
#16329 = VECTOR ( 'NONE', #10518, 1000.000000000000000 ) ;
#16330 = AXIS2_PLACEMENT_3D ( 'NONE', #1384, #17044, #3224 ) ;
#16331 = ORIENTED_EDGE ( 'NONE', *, *, #19716, .F. ) ;
#16332 = VERTEX_POINT ( 'NONE', #20005 ) ;
#16333 = LINE ( 'NONE', #2319, #11833 ) ;
#16334 = B_SPLINE_CURVE_WITH_KNOTS ( 'NONE', 3,
 ( #19080, #15900, #17647, #5066, #12719, #11389, #8013, #18980, #4965, #14260, #5167, #6697, #8316, #3623, #14460, #9849, #2193, #16102, #6597, #1881, #2091, #8421, #12919, #11289 ),
 .UNSPECIFIED., .F., .F.,
 ( 4, 2, 2, 2, 2, 2, 2, 2, 2, 2, 2, 4 ),
 ( 0.05875642544931597433, 0.06915854747235597455, 0.07956066949539594702, 0.08476173050691591937, 0.08736226101267591249, 0.08996279151843590560, 0.1003649135414758364, 0.1107670355645157811, 0.1211691575875557259, 0.1263702185990756843, 0.1315712796105956151, 0.1419734016336355320 ),
 .UNSPECIFIED. ) ;
#16335 = FACE_OUTER_BOUND ( 'NONE', #8937, .T. ) ;
#16336 = DIRECTION ( 'NONE',  ( 1.000000000000000000, 0.000000000000000000, 0.000000000000000000 ) ) ;
#16337 = VERTEX_POINT ( 'NONE', #9373 ) ;
#16338 = DIRECTION ( 'NONE',  ( 1.000000000000000000, 0.000000000000000000, 0.000000000000000000 ) ) ;
#16339 = LINE ( 'NONE', #16042, #6839 ) ;
#16340 = ORIENTED_EDGE ( 'NONE', *, *, #8347, .T. ) ;
#16341 = CARTESIAN_POINT ( 'NONE',  ( 12.28122767885846400, -61.70726652483822505, 248.9926560891072143 ) ) ;
#16342 = DIRECTION ( 'NONE',  ( 1.000000000000000000, 0.000000000000000000, -7.137148015447434001E-15 ) ) ;
#16343 = PLANE ( 'NONE',  #4541 ) ;
#16344 = VECTOR ( 'NONE', #7, 1000.000000000000000 ) ;
#16345 = LINE ( 'NONE', #18170, #2320 ) ;
#16346 = CARTESIAN_POINT ( 'NONE',  ( -135.2402195529228948, -30.09203172481036503, -19.25660886061671562 ) ) ;
#16347 = CARTESIAN_POINT ( 'NONE',  ( 0.4239815141812912636, -0.2650276884262227628, 283.5832628385307999 ) ) ;
#16348 = CARTESIAN_POINT ( 'NONE',  ( -14.39940464655760799, -76.92888220842480962, 112.0427633081292385 ) ) ;
#16349 = ORIENTED_EDGE ( 'NONE', *, *, #6778, .F. ) ;
#16350 = EDGE_CURVE ( 'NONE', #19334, #9538, #7426, .T. ) ;
#16351 = CARTESIAN_POINT ( 'NONE',  ( -13.12769224524071277, -59.30917539369501412, 283.5832628385307999 ) ) ;
#16352 = ORIENTED_EDGE ( 'NONE', *, *, #14398, .F. ) ;
#16353 = VERTEX_POINT ( 'NONE', #9058 ) ;
#16354 = VECTOR ( 'NONE', #7983, 1000.000000000000000 ) ;
#16355 = LINE ( 'NONE', #7045, #9586 ) ;
#16356 = ORIENTED_EDGE ( 'NONE', *, *, #9238, .T. ) ;
#16357 = ORIENTED_EDGE ( 'NONE', *, *, #7524, .F. ) ;
#16358 = ADVANCED_FACE ( 'NONE', ( #9165 ), #6007, .T. ) ;
#16359 = VECTOR ( 'NONE', #17049, 1000.000000000000000 ) ;
#16360 = DIRECTION ( 'NONE',  ( 0.1736481776669306920, -0.9848077530122080203, 0.000000000000000000 ) ) ;
#16361 = ADVANCED_FACE ( 'NONE', ( #10691 ), #13660, .F. ) ;
#16362 = CARTESIAN_POINT ( 'NONE',  ( -84.98223365279403652, -123.6049511534864962, 40.79306686164451889 ) ) ;
#16363 = EDGE_CURVE ( 'NONE', #16204, #11511, #7711, .T. ) ;
#16364 = DIRECTION ( 'NONE',  ( 0.000000000000000000, 0.000000000000000000, 1.000000000000000000 ) ) ;
#16365 = DIRECTION ( 'NONE',  ( -0.000000000000000000, -1.000000000000000000, -0.000000000000000000 ) ) ;
#16366 = EDGE_CURVE ( 'NONE', #13930, #380, #4832, .T. ) ;
#16367 = ORIENTED_EDGE ( 'NONE', *, *, #11850, .T. ) ;
#16368 = CARTESIAN_POINT ( 'NONE',  ( -128.9113527779074388, -76.70395394680458878, 47.60335545142810076 ) ) ;
#16369 = CARTESIAN_POINT ( 'NONE',  ( 97.50000000000001421, -133.9542832461881119, 10.00000000000000178 ) ) ;
#16370 = DIRECTION ( 'NONE',  ( 1.000000000000000000, 0.000000000000000000, 0.000000000000000000 ) ) ;
#16371 = DIRECTION ( 'NONE',  ( -0.3420201433256726542, 0.9396926207859069846, 0.000000000000000000 ) ) ;
#16372 = AXIS2_PLACEMENT_3D ( 'NONE', #8460, #17385, #386 ) ;
#16373 = FACE_OUTER_BOUND ( 'NONE', #17695, .T. ) ;
#16374 = CARTESIAN_POINT ( 'NONE',  ( 159.9599531637113330, -36.50981547336952104, 39.99999999999999289 ) ) ;
#16375 = DIRECTION ( 'NONE',  ( 0.000000000000000000, 0.000000000000000000, -1.000000000000000000 ) ) ;
#16376 = CONICAL_SURFACE ( 'NONE', #11791, 17.50000000000001066, 0.7853981633974479459 ) ;
#16377 = DIRECTION ( 'NONE',  ( 0.000000000000000000, 0.000000000000000000, -1.000000000000000000 ) ) ;
#16378 = ORIENTED_EDGE ( 'NONE', *, *, #15177, .T. ) ;
#16379 = EDGE_CURVE ( 'NONE', #11697, #2515, #4356, .T. ) ;
#16380 = CARTESIAN_POINT ( 'NONE',  ( 0.000000000000000000, 0.000000000000000000, 49.99999999999999289 ) ) ;
#16381 = CARTESIAN_POINT ( 'NONE',  ( -57.61627707419551570, -19.23614321207253042, 293.5832628385307999 ) ) ;
#16382 = ORIENTED_EDGE ( 'NONE', *, *, #4869, .F. ) ;
#16383 = ORIENTED_EDGE ( 'NONE', *, *, #3968, .T. ) ;
#16384 = ITEM_DEFINED_TRANSFORMATION ( 'NONE', 'NONE', #18022,  #18639 ) ;
#16385 = VECTOR ( 'NONE', #18550, 1000.000000000000000 ) ;
#16386 = EDGE_CURVE ( 'NONE', #16400, #3088, #18852, .T. ) ;
#16387 = DIRECTION ( 'NONE',  ( -0.000000000000000000, -0.000000000000000000, -1.000000000000000000 ) ) ;
#16388 = ORIENTED_EDGE ( 'NONE', *, *, #16121, .T. ) ;
#16389 = EDGE_CURVE ( 'NONE', #12180, #55, #4256, .T. ) ;
#16390 = CIRCLE ( 'NONE', #7219, 17.50000000000000355 ) ;
#16391 = CARTESIAN_POINT ( 'NONE',  ( 90.38423273154630522, -119.7175801288824317, -6.689658229812266654 ) ) ;
#16392 = CARTESIAN_POINT ( 'NONE',  ( -85.51233150139636052, -123.2383548749651538, -1.612964112344334344 ) ) ;
#16393 = EDGE_CURVE ( 'NONE', #20158, #16054, #9272, .T. ) ;
#16394 = CARTESIAN_POINT ( 'NONE',  ( -84.00455766787156620, -124.2712478689755642, 1.041419029133151097 ) ) ;
#16395 = FACE_OUTER_BOUND ( 'NONE', #9198, .T. ) ;
#16396 = CARTESIAN_POINT ( 'NONE',  ( 11.54977938102087620, -57.55901709132175625, 112.0427633081291816 ) ) ;
#16397 = LINE ( 'NONE', #18122, #17428 ) ;
#16398 = FACE_OUTER_BOUND ( 'NONE', #4940, .T. ) ;
#16399 = CARTESIAN_POINT ( 'NONE',  ( 59.42266395395792955, -50.93469132750283279, 132.4711112102474146 ) ) ;
#16400 = VERTEX_POINT ( 'NONE', #12325 ) ;
#16401 = ADVANCED_FACE ( 'NONE', ( #17052 ), #18586, .F. ) ;
#16402 = CARTESIAN_POINT ( 'NONE',  ( -110.0000000000000142, 285.0000000000000568, 5.000000000000000888 ) ) ;
#16403 = LINE ( 'NONE', #2581, #13450 ) ;
#16404 = ORIENTED_EDGE ( 'NONE', *, *, #1615, .T. ) ;
#16405 = AXIS2_PLACEMENT_3D ( 'NONE', #6310, #12427, #12317 ) ;
#16406 = ORIENTED_EDGE ( 'NONE', *, *, #18932, .F. ) ;
#16407 = CARTESIAN_POINT ( 'NONE',  ( -44.79787735033389851, 41.02212542604627998, 293.5832628385307999 ) ) ;
#16408 = ORIENTED_EDGE ( 'NONE', *, *, #17980, .T. ) ;
#16409 = ADVANCED_FACE ( 'NONE', ( #19803 ), #3039, .F. ) ;
#16410 = EDGE_CURVE ( 'NONE', #2269, #9812, #17867, .T. ) ;
#16411 = CARTESIAN_POINT ( 'NONE',  ( -0.8220851292435327196, -78.26059000578311498, 132.4711112102474146 ) ) ;
#16412 = EDGE_CURVE ( 'NONE', #2109, #16031, #7728, .T. ) ;
#16413 = EDGE_CURVE ( 'NONE', #6462, #13002, #18177, .T. ) ;
#16414 = LINE ( 'NONE', #3529, #18115 ) ;
#16415 = CARTESIAN_POINT ( 'NONE',  ( 63.68887634719569490, -147.8252249328912740, 60.00000000000000000 ) ) ;
#16416 = CARTESIAN_POINT ( 'NONE',  ( -74.01264520835137262, 25.47058595421628269, 111.4180192758973931 ) ) ;
#16417 = DIRECTION ( 'NONE',  ( -1.000000000000000000, 0.000000000000000000, 0.000000000000000000 ) ) ;
#16418 = LINE ( 'NONE', #19290, #10409 ) ;
#16419 = CARTESIAN_POINT ( 'NONE',  ( -127.3324793557758596, -79.33838548637069721, -0.8616620075509384691 ) ) ;
#16420 = CARTESIAN_POINT ( 'NONE',  ( 135.0085555318104866, -65.36720921928018413, 6.996239623563403676 ) ) ;
#16421 = VECTOR ( 'NONE', #11587, 1000.000000000000227 ) ;
#16422 = EDGE_CURVE ( 'NONE', #14351, #14876, #3507, .T. ) ;
#16423 = VECTOR ( 'NONE', #14752, 1000.000000000000000 ) ;
#16424 = DIRECTION ( 'NONE',  ( 0.000000000000000000, 0.000000000000000000, -1.000000000000000000 ) ) ;
#16425 = CARTESIAN_POINT ( 'NONE',  ( -79.75827554147308263, 9.767571684737763671E-15, 132.4711112102474146 ) ) ;
#16426 = ORIENTED_EDGE ( 'NONE', *, *, #605, .F. ) ;
#16427 = CIRCLE ( 'NONE', #4998, 62.91752772691707207 ) ;
#16428 = VECTOR ( 'NONE', #4100, 1000.000000000000114 ) ;
#16429 = ORIENTED_EDGE ( 'NONE', *, *, #10136, .F. ) ;
#16430 = ORIENTED_EDGE ( 'NONE', *, *, #19701, .F. ) ;
#16431 = ORIENTED_EDGE ( 'NONE', *, *, #999, .T. ) ;
#16432 = DIRECTION ( 'NONE',  ( -0.6234898018587431423, 0.7818314824680221431, 0.000000000000000000 ) ) ;
#16433 = AXIS2_PLACEMENT_3D ( 'NONE', #8086, #15877, #14440 ) ;
#16434 = CIRCLE ( 'NONE', #8260, 7.500000000000012434 ) ;
#16435 = ORIENTED_EDGE ( 'NONE', *, *, #15997, .F. ) ;
#16436 = CARTESIAN_POINT ( 'NONE',  ( 17.24542129382117750, 20.55229278271219329, 14.88498244535533033 ) ) ;
#16437 = FACE_BOUND ( 'NONE', #18701, .T. ) ;
#16438 = DIRECTION ( 'NONE',  ( -0.000000000000000000, -0.000000000000000000, -1.000000000000000000 ) ) ;
#16439 = EDGE_LOOP ( 'NONE', ( #9059, #2335, #6631, #9256 ) ) ;
#16440 = AXIS2_PLACEMENT_3D ( 'NONE', #13771, #15309, #4467 ) ;
#16441 = DIRECTION ( 'NONE',  ( -0.000000000000000000, -0.000000000000000000, 1.000000000000000000 ) ) ;
#16442 = PLANE ( 'NONE',  #939 ) ;
#16443 = EDGE_CURVE ( 'NONE', #11539, #1303, #17159, .T. ) ;
#16444 = ORIENTED_EDGE ( 'NONE', *, *, #9144, .T. ) ;
#16445 = DIRECTION ( 'NONE',  ( 0.000000000000000000, 0.000000000000000000, 1.000000000000000000 ) ) ;
#16446 = CARTESIAN_POINT ( 'NONE',  ( -141.8714406926361562, -48.70825716237266079, 60.00000000000000000 ) ) ;
#16447 = CARTESIAN_POINT ( 'NONE',  ( -134.6433994324794412, -73.52870175801841413, 7.634837572223202251 ) ) ;
#16448 = CARTESIAN_POINT ( 'NONE',  ( 49.24833719034187851, 60.83768308848395634, 132.4711112102474146 ) ) ;
#16449 = VECTOR ( 'NONE', #1322, 1000.000000000000000 ) ;
#16450 = VECTOR ( 'NONE', #8548, 1000.000000000000000 ) ;
#16451 = CARTESIAN_POINT ( 'NONE',  ( 112.4320812185964371, -22.51277856475483574, 39.88498244535466597 ) ) ;
#16452 = DIRECTION ( 'NONE',  ( 0.4999999999999916178, -0.8660254037844435926, -4.304393070272782536E-15 ) ) ;
#16453 = VERTEX_POINT ( 'NONE', #4983 ) ;
#16454 = CARTESIAN_POINT ( 'NONE',  ( 0.000000000000000000, 0.000000000000000000, 293.5832628385307999 ) ) ;
#16455 = ORIENTED_EDGE ( 'NONE', *, *, #9118, .T. ) ;
#16456 = VECTOR ( 'NONE', #13975, 999.9999999999998863 ) ;
#16457 = ORIENTED_EDGE ( 'NONE', *, *, #11824, .F. ) ;
#16458 = DIRECTION ( 'NONE',  ( -1.613511099790691498E-16, 1.000000000000000000, 0.000000000000000000 ) ) ;
#16459 = VECTOR ( 'NONE', #1116, 1000.000000000000227 ) ;
#16460 = VERTEX_POINT ( 'NONE', #6416 ) ;
#16461 = LINE ( 'NONE', #18185, #12680 ) ;
#16462 = CARTESIAN_POINT ( 'NONE',  ( 0.000000000000000000, 0.000000000000000000, 293.5832628385307999 ) ) ;
#16463 = VECTOR ( 'NONE', #19513, 1000.000000000000000 ) ;
#16464 = DIRECTION ( 'NONE',  ( 1.000000000000000000, 0.000000000000000000, 0.000000000000000000 ) ) ;
#16465 = CARTESIAN_POINT ( 'NONE',  ( 159.9599531637113330, -36.50981547336952104, 39.99999999999999289 ) ) ;
#16466 = EDGE_CURVE ( 'NONE', #5287, #7766, #14901, .T. ) ;
#16467 = ORIENTED_EDGE ( 'NONE', *, *, #13371, .T. ) ;
#16468 = DIRECTION ( 'NONE',  ( 1.000000000000000000, 0.000000000000000000, 0.000000000000000000 ) ) ;
#16469 = DIRECTION ( 'NONE',  ( 1.000000000000000000, 0.000000000000000000, 0.000000000000000000 ) ) ;
#16470 = AXIS2_PLACEMENT_3D ( 'NONE', #8104, #442, #19170 ) ;
#16471 = DIRECTION ( 'NONE',  ( 0.000000000000000000, 0.000000000000000000, 1.000000000000000000 ) ) ;
#16472 = CARTESIAN_POINT ( 'NONE',  ( 18.28567271940513450, -57.92709869106715814, 293.5832628385307999 ) ) ;
#16473 = ORIENTED_EDGE ( 'NONE', *, *, #6394, .T. ) ;
#16474 = VECTOR ( 'NONE', #4688, 1000.000000000000000 ) ;
#16475 = LINE ( 'NONE', #3885, #2851 ) ;
#16476 = CYLINDRICAL_SURFACE ( 'NONE', #12754, 9.999999999999994671 ) ;
#16477 = PLANE ( 'NONE',  #2706 ) ;
#16478 = VERTEX_POINT ( 'NONE', #64 ) ;
#16479 = EDGE_CURVE ( 'NONE', #11921, #13055, #9358, .T. ) ;
#16480 = DIRECTION ( 'NONE',  ( 1.000000000000000000, 0.000000000000000000, 0.000000000000000000 ) ) ;
#16481 = CARTESIAN_POINT ( 'NONE',  ( 0.000000000000000000, 0.000000000000000000, 283.5832628385307999 ) ) ;
#16482 = EDGE_LOOP ( 'NONE', ( #18857, #4575, #6785, #15764 ) ) ;
#16483 = ORIENTED_EDGE ( 'NONE', *, *, #18991, .F. ) ;
#16484 = ORIENTED_EDGE ( 'NONE', *, *, #19364, .T. ) ;
#16485 = CARTESIAN_POINT ( 'NONE',  ( -29.99999999999887379, 285.0000000000000568, 12.49999999999916511 ) ) ;
#16486 = DIRECTION ( 'NONE',  ( -0.9009688679024219216, 0.4338837391175523472, 0.000000000000000000 ) ) ;
#16487 = CIRCLE ( 'NONE', #14837, 7.500000000000003553 ) ;
#16488 = ORIENTED_EDGE ( 'NONE', *, *, #19520, .T. ) ;
#16489 = CARTESIAN_POINT ( 'NONE',  ( 106.9434277525946868, -119.5160896407720941, -3.835367999719689524E-15 ) ) ;
#16490 = CARTESIAN_POINT ( 'NONE',  ( -93.97987429417752026, -116.9112352313915295, -8.647211263555981020 ) ) ;
#16491 = EDGE_CURVE ( 'NONE', #4614, #8547, #3165, .T. ) ;
#16492 = CARTESIAN_POINT ( 'NONE',  ( -139.9227089858103454, -5.347203697601174532, 23.15800849071695922 ) ) ;
#16493 = DIRECTION ( 'NONE',  ( 0.7430374143461878633, -0.6692498792541777819, 0.000000000000000000 ) ) ;
#16494 = CARTESIAN_POINT ( 'NONE',  ( 3.453261854573022482, 4.581103194070020201, 293.5832628385307999 ) ) ;
#16495 = CARTESIAN_POINT ( 'NONE',  ( -29.99999999999887379, 275.0000000000000000, -2.500000000000847766 ) ) ;
#16496 = CIRCLE ( 'NONE', #4407, 79.75827554147308263 ) ;
#16497 = CARTESIAN_POINT ( 'NONE',  ( 59.06449708980161972, 51.36153797460926995, 132.4711112102474146 ) ) ;
#16498 = DIRECTION ( 'NONE',  ( -1.000000000000000000, 0.000000000000000000, 0.000000000000000000 ) ) ;
#16499 = DIRECTION ( 'NONE',  ( 0.000000000000000000, 0.000000000000000000, 1.000000000000000000 ) ) ;
#16500 = ORIENTED_EDGE ( 'NONE', *, *, #9749, .F. ) ;
#16501 = ADVANCED_FACE ( 'NONE', ( #11101 ), #3337, .T. ) ;
#16502 = CARTESIAN_POINT ( 'NONE',  ( 7.350000000000000533, 5.196152422706624030, -9.000000000000001776 ) ) ;
#16503 = CARTESIAN_POINT ( 'NONE',  ( 7.500000000000001776, 60.00000000000000000, -105.0000000000000142 ) ) ;
#16504 = EDGE_CURVE ( 'NONE', #18380, #14190, #10049, .T. ) ;
#16505 = ORIENTED_EDGE ( 'NONE', *, *, #5262, .F. ) ;
#16506 = AXIS2_PLACEMENT_3D ( 'NONE', #16856, #2849, #7152 ) ;
#16507 = ORIENTED_EDGE ( 'NONE', *, *, #5756, .T. ) ;
#16508 = CARTESIAN_POINT ( 'NONE',  ( -0.8220851292435327196, -78.26059000578311498, 248.9926560891072143 ) ) ;
#16509 = ORIENTED_EDGE ( 'NONE', *, *, #9627, .F. ) ;
#16510 = AXIS2_PLACEMENT_3D ( 'NONE', #10056, #16307, #2290 ) ;
#16511 = CARTESIAN_POINT ( 'NONE',  ( 130.9868171408399462, -91.88282611735539263, 0.000000000000000000 ) ) ;
#16512 = EDGE_CURVE ( 'NONE', #7714, #2316, #17467, .T. ) ;
#16513 = CARTESIAN_POINT ( 'NONE',  ( 0.000000000000000000, 0.000000000000000000, 60.00000000000000000 ) ) ;
#16514 = CARTESIAN_POINT ( 'NONE',  ( -99.73767742490161936, -112.0463336856493299, 50.00000000005213963 ) ) ;
#16515 = CARTESIAN_POINT ( 'NONE',  ( -60.22029172860436574, -7.948651060879222463, 293.5832628385307999 ) ) ;
#16516 = ORIENTED_EDGE ( 'NONE', *, *, #10144, .F. ) ;
#16517 = PLANE ( 'NONE',  #9457 ) ;
#16518 = DIRECTION ( 'NONE',  ( 0.000000000000000000, 0.000000000000000000, 1.000000000000000000 ) ) ;
#16519 = DIRECTION ( 'NONE',  ( -0.8660254037844328234, -0.5000000000000101030, -0.000000000000000000 ) ) ;
#16520 = DIRECTION ( 'NONE',  ( -0.1736481776669408228, -0.9848077530122062440, 1.076098267568195042E-15 ) ) ;
#16521 = DIRECTION ( 'NONE',  ( -0.2225209339563057609, -0.9749279121818256177, 0.000000000000000000 ) ) ;
#16522 = CARTESIAN_POINT ( 'NONE',  ( -132.9399949862640824, -69.60197982539851580, 33.36755373876824393 ) ) ;
#16523 = ORIENTED_EDGE ( 'NONE', *, *, #5904, .F. ) ;
#16524 = EDGE_CURVE ( 'NONE', #15095, #13722, #1906, .T. ) ;
#16525 = EDGE_CURVE ( 'NONE', #998, #2414, #16028, .T. ) ;
#16526 = ADVANCED_FACE ( 'NONE', ( #14481 ), #9871, .T. ) ;
#16527 = ORIENTED_EDGE ( 'NONE', *, *, #8135, .F. ) ;
#16528 = ORIENTED_EDGE ( 'NONE', *, *, #7093, .T. ) ;
#16529 = AXIS2_PLACEMENT_3D ( 'NONE', #7220, #6829, #10372 ) ;
#16530 = VERTEX_POINT ( 'NONE', #1603 ) ;
#16531 = EDGE_LOOP ( 'NONE', ( #11489, #10109, #2518 ) ) ;
#16532 = VECTOR ( 'NONE', #2848, 1000.000000000000000 ) ;
#16533 = CARTESIAN_POINT ( 'NONE',  ( 59.42266395395792955, -50.93469132750283279, 248.9926560891072143 ) ) ;
#16534 = EDGE_CURVE ( 'NONE', #15414, #739, #7831, .T. ) ;
#16535 = LINE ( 'NONE', #10278, #13853 ) ;
#16536 = LINE ( 'NONE', #10182, #5471 ) ;
#16537 = EDGE_LOOP ( 'NONE', ( #10112, #7611, #6400, #15577 ) ) ;
#16538 = DIRECTION ( 'NONE',  ( 1.000000000000000000, 0.000000000000000000, 0.000000000000000000 ) ) ;
#16539 = DIRECTION ( 'NONE',  ( 0.000000000000000000, 0.000000000000000000, 1.000000000000000000 ) ) ;
#16540 = ORIENTED_EDGE ( 'NONE', *, *, #18405, .F. ) ;
#16541 = CARTESIAN_POINT ( 'NONE',  ( 0.000000000000000000, 0.000000000000000000, 132.4711112102474146 ) ) ;
#16542 = CARTESIAN_POINT ( 'NONE',  ( 67.50000000000000000, 6.284666409917639535E-13, -115.0000000000000000 ) ) ;
#16543 = CARTESIAN_POINT ( 'NONE',  ( -150.0000000000000284, 0.000000000000000000, -10.00000000000000178 ) ) ;
#16544 = DIRECTION ( 'NONE',  ( -0.000000000000000000, -0.000000000000000000, -1.000000000000000000 ) ) ;
#16545 = VECTOR ( 'NONE', #18663, 1000.000000000000000 ) ;
#16546 = VECTOR ( 'NONE', #15522, 1000.000000000000000 ) ;
#16547 = EDGE_CURVE ( 'NONE', #274, #14568, #15718, .T. ) ;
#16548 = CARTESIAN_POINT ( 'NONE',  ( -59.42266395395758138, 50.93469132750324491, 248.9926560891072143 ) ) ;
#16549 = CARTESIAN_POINT ( 'NONE',  ( 1.396592535537252080E-14, 0.000000000000000000, 49.99999999999998579 ) ) ;
#16550 = EDGE_LOOP ( 'NONE', ( #16126, #14913, #9979, #281, #3570, #12635 ) ) ;
#16551 = AXIS2_PLACEMENT_3D ( 'NONE', #17787, #5698, #3954 ) ;
#16552 = CARTESIAN_POINT ( 'NONE',  ( 7.950000000000000178, -5.196152422706636465, -8.999999999999998224 ) ) ;
#16553 = ORIENTED_EDGE ( 'NONE', *, *, #1543, .F. ) ;
#16554 = ADVANCED_FACE ( 'NONE', ( #2983 ), #8901, .F. ) ;
#16555 = DIRECTION ( 'NONE',  ( -1.000000000000000000, -0.000000000000000000, -0.000000000000000000 ) ) ;
#16556 = VERTEX_POINT ( 'NONE', #12380 ) ;
#16557 = ORIENTED_EDGE ( 'NONE', *, *, #9353, .F. ) ;
#16558 = VECTOR ( 'NONE', #19598, 1000.000000000000000 ) ;
#16559 = CARTESIAN_POINT ( 'NONE',  ( 138.2024300533213932, 89.85329105948596862, 39.99999999999999289 ) ) ;
#16560 = VECTOR ( 'NONE', #4088, 1000.000000000000000 ) ;
#16561 = CARTESIAN_POINT ( 'NONE',  ( -83.87053960371946459, -124.3614079552663441, 38.64581828052915569 ) ) ;
#16562 = FACE_OUTER_BOUND ( 'NONE', #5395, .T. ) ;
#16563 = DIRECTION ( 'NONE',  ( 0.000000000000000000, -0.000000000000000000, -1.000000000000000000 ) ) ;
#16564 = ORIENTED_EDGE ( 'NONE', *, *, #15623, .F. ) ;
#16565 = CIRCLE ( 'NONE', #13284, 15.91767397667355155 ) ;
#16566 = CARTESIAN_POINT ( 'NONE',  ( -135.1060089022256818, -65.16414933467417825, 30.00000000000000000 ) ) ;
#16567 = DIRECTION ( 'NONE',  ( 0.000000000000000000, 0.000000000000000000, -1.000000000000000000 ) ) ;
#16568 = CARTESIAN_POINT ( 'NONE',  ( -0.8220851292435327196, -62.91215678473957240, 293.5832628385307999 ) ) ;
#16569 = CARTESIAN_POINT ( 'NONE',  ( 0.000000000000000000, 0.000000000000000000, -9.999999999999987566 ) ) ;
#16570 = ORIENTED_EDGE ( 'NONE', *, *, #19389, .T. ) ;
#16571 = FACE_OUTER_BOUND ( 'NONE', #18650, .T. ) ;
#16572 = LINE ( 'NONE', #11839, #19932 ) ;
#16573 = DIRECTION ( 'NONE',  ( -1.000000000000000000, -1.047444401652940164E-14, 0.000000000000000000 ) ) ;
#16574 = ORIENTED_EDGE ( 'NONE', *, *, #15882, .F. ) ;
#16575 = DIRECTION ( 'NONE',  ( 0.6692498792541753394, 0.7430374143461900838, 0.000000000000000000 ) ) ;
#16576 = DIRECTION ( 'NONE',  ( 1.000000000000000000, 0.000000000000000000, 0.000000000000000000 ) ) ;
#16577 = ORIENTED_EDGE ( 'NONE', *, *, #1932, .F. ) ;
#16578 = ORIENTED_EDGE ( 'NONE', *, *, #5787, .T. ) ;
#16579 = VECTOR ( 'NONE', #7957, 1000.000000000000000 ) ;
#16580 = CIRCLE ( 'NONE', #8071, 62.91752772691707207 ) ;
#16581 = DIRECTION ( 'NONE',  ( -6.982962677686266711E-15, 0.000000000000000000, -1.000000000000000000 ) ) ;
#16582 = DIRECTION ( 'NONE',  ( -0.4338837391175523472, -0.9009688679024219216, 0.000000000000000000 ) ) ;
#16583 = ORIENTED_EDGE ( 'NONE', *, *, #14138, .F. ) ;
#16584 = CYLINDRICAL_SURFACE ( 'NONE', #3449, 40.00000000000000711 ) ;
#16585 = DIRECTION ( 'NONE',  ( 0.000000000000000000, 0.000000000000000000, -1.000000000000000000 ) ) ;
#16586 = CIRCLE ( 'NONE', #11671, 62.91752772691707207 ) ;
#16587 = CARTESIAN_POINT ( 'NONE',  ( 11.00103590902871353, 57.65577537092163851, 132.4711112102474146 ) ) ;
#16588 = VECTOR ( 'NONE', #14998, 999.9999999999998863 ) ;
#16589 = CARTESIAN_POINT ( 'NONE',  ( 81.66698895276879000, 79.37254397626031732, 14.88498244535488269 ) ) ;
#16590 = CARTESIAN_POINT ( 'NONE',  ( -14.94814811854910452, 76.83212392882506947, 248.9926560891072143 ) ) ;
#16591 = CARTESIAN_POINT ( 'NONE',  ( -0.2993243175131807821, 5.729042578294318844, 293.5832628385307999 ) ) ;
#16592 = CYLINDRICAL_SURFACE ( 'NONE', #18391, 3.224098631618460331 ) ;
#16593 = EDGE_LOOP ( 'NONE', ( #16676, #4257, #18709, #3925, #1863, #5668 ) ) ;
#16594 = DIRECTION ( 'NONE',  ( -6.982962677686266711E-15, 0.000000000000000000, -1.000000000000000000 ) ) ;
#16595 = CARTESIAN_POINT ( 'NONE',  ( -63.98537287693041264, 94.20918150411493741, 14.88498244535589876 ) ) ;
#16596 = VERTEX_POINT ( 'NONE', #7676 ) ;
#16597 = ADVANCED_FACE ( 'NONE', ( #9211 ), #4203, .T. ) ;
#16598 = VERTEX_POINT ( 'NONE', #13915 ) ;
#16599 = ORIENTED_EDGE ( 'NONE', *, *, #15915, .T. ) ;
#16600 = AXIS2_PLACEMENT_3D ( 'NONE', #1209, #12150, #18411 ) ;
#16601 = CARTESIAN_POINT ( 'NONE',  ( 45.48770046196260353, 37.09555676057011908, 248.9926560891072143 ) ) ;
#16602 = ORIENTED_EDGE ( 'NONE', *, *, #8168, .T. ) ;
#16603 = EDGE_CURVE ( 'NONE', #4103, #14479, #15146, .T. ) ;
#16604 = CARTESIAN_POINT ( 'NONE',  ( 131.9731329243527398, -88.11278280481133152, 0.2335709844691223058 ) ) ;
#16605 = FACE_OUTER_BOUND ( 'NONE', #19957, .T. ) ;
#16606 = CARTESIAN_POINT ( 'NONE',  ( -25.74015858913164578, 7.810105800529631992, 14.88498244535563231 ) ) ;
#16607 = ADVANCED_FACE ( 'NONE', ( #4408 ), #7370, .F. ) ;
#16608 = CARTESIAN_POINT ( 'NONE',  ( -106.3851141486743188, -120.5004170265707444, 39.95383784551692941 ) ) ;
#16609 = EDGE_CURVE ( 'NONE', #1203, #19359, #8400, .T. ) ;
#16610 = PLANE ( 'NONE',  #4441 ) ;
#16611 = CARTESIAN_POINT ( 'NONE',  ( 57.92709869106709419, 18.28567271940532990, 283.5832628385307999 ) ) ;
#16612 = VERTEX_POINT ( 'NONE', #13812 ) ;
#16613 = EDGE_CURVE ( 'NONE', #166, #9431, #3235, .T. ) ;
#16614 = CYLINDRICAL_SURFACE ( 'NONE', #8784, 15.91767397667354089 ) ;
#16615 = CARTESIAN_POINT ( 'NONE',  ( -128.0922826834541297, -78.05640312850694329, -8.225544806820535015 ) ) ;
#16616 = DIRECTION ( 'NONE',  ( 0.7660444431189771253, 0.6427876096865405842, 0.000000000000000000 ) ) ;
#16617 = CIRCLE ( 'NONE', #10387, 60.74260934110282051 ) ;
#16618 = DIRECTION ( 'NONE',  ( 1.000000000000000000, 0.000000000000000000, -6.994638739193269649E-15 ) ) ;
#16619 = FACE_OUTER_BOUND ( 'NONE', #12917, .T. ) ;
#16620 = CIRCLE ( 'NONE', #5194, 60.74260934110282051 ) ;
#16621 = CARTESIAN_POINT ( 'NONE',  ( -1.678175111358135130, -5.485913980968154746, 283.5832628385307999 ) ) ;
#16622 = EDGE_LOOP ( 'NONE', ( #8828, #7261, #12446, #7153 ) ) ;
#16623 = AXIS2_PLACEMENT_3D ( 'NONE', #7922, #10991, #3227 ) ;
#16624 = EDGE_CURVE ( 'NONE', #2833, #19796, #15588, .T. ) ;
#16625 = ORIENTED_EDGE ( 'NONE', *, *, #19400, .F. ) ;
#16626 = EDGE_LOOP ( 'NONE', ( #19940, #14004 ) ) ;
#16627 = VERTEX_POINT ( 'NONE', #19951 ) ;
#16628 = ORIENTED_EDGE ( 'NONE', *, *, #860, .T. ) ;
#16629 = CIRCLE ( 'NONE', #8126, 106.4288957539800862 ) ;
#16630 = VECTOR ( 'NONE', #3559, 1000.000000000000114 ) ;
#16631 = LINE ( 'NONE', #5889, #4381 ) ;
#16632 = CARTESIAN_POINT ( 'NONE',  ( -97.49999999999997158, -190.0000000000000000, 30.00000000000000000 ) ) ;
#16633 = ORIENTED_EDGE ( 'NONE', *, *, #6814, .F. ) ;
#16634 = EDGE_CURVE ( 'NONE', #6667, #8663, #6112, .T. ) ;
#16635 = CARTESIAN_POINT ( 'NONE',  ( 0.000000000000000000, -7.794228634059936489, 4.500000000000017764 ) ) ;
#16636 = DIRECTION ( 'NONE',  ( 6.982962677686266711E-15, -0.000000000000000000, 1.000000000000000000 ) ) ;
#16637 = EDGE_CURVE ( 'NONE', #7405, #3935, #16690, .T. ) ;
#16638 = ORIENTED_EDGE ( 'NONE', *, *, #15684, .F. ) ;
#16639 = CARTESIAN_POINT ( 'NONE',  ( -159.9599531637108782, -36.50981547337168109, 39.99999999999999289 ) ) ;
#16640 = CARTESIAN_POINT ( 'NONE',  ( -41.02212542604613787, -44.79787735033403351, 283.5832628385307999 ) ) ;
#16641 = CARTESIAN_POINT ( 'NONE',  ( -134.5752827950141466, -74.04736996659983106, 6.800259422634988837 ) ) ;
#16642 = CARTESIAN_POINT ( 'NONE',  ( -77.21438937758510690, -12.78021302872823384, 248.9926560891072143 ) ) ;
#16643 = CARTESIAN_POINT ( 'NONE',  ( 126.7530218919796567, -80.25302646197467027, 40.98242217817278998 ) ) ;
#16644 = DIRECTION ( 'NONE',  ( -6.982962677686266711E-15, 0.000000000000000000, -1.000000000000000000 ) ) ;
#16645 = VECTOR ( 'NONE', #14931, 1000.000000000000114 ) ;
#16646 = AXIS2_PLACEMENT_3D ( 'NONE', #15065, #7293, #10165 ) ;
#16647 = VERTEX_POINT ( 'NONE', #10531 ) ;
#16648 = ADVANCED_FACE ( 'NONE', ( #9003 ), #15244, .T. ) ;
#16649 = FACE_OUTER_BOUND ( 'NONE', #13362, .T. ) ;
#16650 = ORIENTED_EDGE ( 'NONE', *, *, #1218, .F. ) ;
#16651 = ORIENTED_EDGE ( 'NONE', *, *, #13114, .T. ) ;
#16652 = FACE_OUTER_BOUND ( 'NONE', #17008, .T. ) ;
#16653 = ORIENTED_EDGE ( 'NONE', *, *, #7524, .T. ) ;
#16654 = ORIENTED_EDGE ( 'NONE', *, *, #9464, .T. ) ;
#16655 = CARTESIAN_POINT ( 'NONE',  ( -53.78543575132152199, -32.64570716507522263, 248.9926560891072143 ) ) ;
#16656 = SURFACE_STYLE_USAGE ( .BOTH. , #18187 ) ;
#16657 = CARTESIAN_POINT ( 'NONE',  ( 100.7812500000000000, -111.0996833858562525, 49.99999999999999289 ) ) ;
#16658 = EDGE_CURVE ( 'NONE', #9091, #648, #10672, .T. ) ;
#16659 = CARTESIAN_POINT ( 'NONE',  ( 14.39940464655707331, 76.92888220842492331, 132.4711112102474146 ) ) ;
#16660 = CARTESIAN_POINT ( 'NONE',  ( 38.41834839689379777, -68.18670162478818497, 110.9660488491356887 ) ) ;
#16661 = ADVANCED_FACE ( 'NONE', ( #18431 ), #18528, .T. ) ;
#16662 = ORIENTED_EDGE ( 'NONE', *, *, #15024, .T. ) ;
#16663 = CARTESIAN_POINT ( 'NONE',  ( -9.564549117045519466, -62.18629025319811632, 248.9926560891072143 ) ) ;
#16664 = CYLINDRICAL_SURFACE ( 'NONE', #14664, 7.500000000000020428 ) ;
#16665 = ADVANCED_FACE ( 'NONE', ( #4510, #10633 ), #15348, .T. ) ;
#16666 = DIRECTION ( 'NONE',  ( -0.000000000000000000, -0.000000000000000000, 1.000000000000000000 ) ) ;
#16667 = EDGE_LOOP ( 'NONE', ( #17633, #8244, #15699, #6644 ) ) ;
#16668 = CARTESIAN_POINT ( 'NONE',  ( 0.000000000000000000, 0.000000000000000000, 283.5832628385307999 ) ) ;
#16669 = CARTESIAN_POINT ( 'NONE',  ( -17.49999999999999289, 0.000000000000000000, 60.00000000000000000 ) ) ;
#16670 = CARTESIAN_POINT ( 'NONE',  ( 11.54085525628718401, 113.2974248684783163, 14.88498244535537296 ) ) ;
#16671 = VERTEX_POINT ( 'NONE', #16997 ) ;
#16672 = AXIS2_PLACEMENT_3D ( 'NONE', #14436, #6670, #9624 ) ;
#16673 = DIRECTION ( 'NONE',  ( 0.000000000000000000, 0.000000000000000000, 1.000000000000000000 ) ) ;
#16674 = LINE ( 'NONE', #1108, #1074 ) ;
#16675 = AXIS2_PLACEMENT_3D ( 'NONE', #7891, #6066, #12391 ) ;
#16676 = ORIENTED_EDGE ( 'NONE', *, *, #17739, .F. ) ;
#16677 = AXIS2_PLACEMENT_3D ( 'NONE', #8803, #4612, #5843 ) ;
#16678 = VERTEX_POINT ( 'NONE', #16075 ) ;
#16679 = CARTESIAN_POINT ( 'NONE',  ( -82.42180963433014540, -125.3261898519405548, 34.07777747112352529 ) ) ;
#16680 = ORIENTED_EDGE ( 'NONE', *, *, #16603, .F. ) ;
#16681 = DIRECTION ( 'NONE',  ( -0.7660444431189813441, 0.6427876096865353661, 0.000000000000000000 ) ) ;
#16682 = CARTESIAN_POINT ( 'NONE',  ( -78.26059000578311498, -1.379293853802028291, 112.7772637782949516 ) ) ;
#16683 = ORIENTED_EDGE ( 'NONE', *, *, #10379, .T. ) ;
#16684 = CARTESIAN_POINT ( 'NONE',  ( 95.54273718349524813, -115.6434791701545493, -9.240355742637868630 ) ) ;
#16685 = CARTESIAN_POINT ( 'NONE',  ( -96.59694518724896284, -114.7646842535148437, -9.528509010735914941 ) ) ;
#16686 = VECTOR ( 'NONE', #17091, 1000.000000000000000 ) ;
#16687 = EDGE_CURVE ( 'NONE', #16956, #9432, #11001, .T. ) ;
#16688 = DIRECTION ( 'NONE',  ( -0.000000000000000000, -0.000000000000000000, 1.000000000000000000 ) ) ;
#16689 = CARTESIAN_POINT ( 'NONE',  ( 0.000000000000000000, 0.000000000000000000, -115.0000000000000000 ) ) ;
#16690 = LINE ( 'NONE', #3085, #1537 ) ;
#16691 = DIRECTION ( 'NONE',  ( -0.000000000000000000, -0.000000000000000000, 1.000000000000000000 ) ) ;
#16692 = LINE ( 'NONE', #11768, #17414 ) ;
#16693 = ORIENTED_EDGE ( 'NONE', *, *, #9616, .T. ) ;
#16694 = DIRECTION ( 'NONE',  ( 0.7660444431189749048, 0.6427876096865430267, 0.000000000000000000 ) ) ;
#16695 = DIRECTION ( 'NONE',  ( -0.000000000000000000, -0.000000000000000000, 1.000000000000000000 ) ) ;
#16696 = ORIENTED_EDGE ( 'NONE', *, *, #16048, .F. ) ;
#16697 = AXIS2_PLACEMENT_3D ( 'NONE', #10795, #17050, #13760 ) ;
#16698 = ORIENTED_EDGE ( 'NONE', *, *, #480, .F. ) ;
#16699 =( NAMED_UNIT ( * ) PLANE_ANGLE_UNIT ( ) SI_UNIT ( $, .RADIAN. ) );
#16700 = AXIS2_PLACEMENT_3D ( 'NONE', #4855, #1778, #14360 ) ;
#16701 = VERTEX_POINT ( 'NONE', #7982 ) ;
#16702 = CARTESIAN_POINT ( 'NONE',  ( -127.4413876050234364, 1.560706874093891490E-14, 43.88498244535634285 ) ) ;
#16703 = ORIENTED_EDGE ( 'NONE', *, *, #3905, .F. ) ;
#16704 = CARTESIAN_POINT ( 'NONE',  ( 134.6416478978700013, -73.54075392783713028, 7.639997785598048097 ) ) ;
#16705 = CARTESIAN_POINT ( 'NONE',  ( 41.48948842197119546, -47.29944656917769663, 132.4711112102474146 ) ) ;
#16706 = CARTESIAN_POINT ( 'NONE',  ( -8.833100819207983179, -58.03804081968163331, 112.0427633081292385 ) ) ;
#16707 = LINE ( 'NONE', #13416, #18927 ) ;
#16708 = DIRECTION ( 'NONE',  ( 0.000000000000000000, 0.000000000000000000, -1.000000000000000000 ) ) ;
#16709 = ADVANCED_FACE ( 'NONE', ( #19144 ), #110, .T. ) ;
#16710 = VERTEX_POINT ( 'NONE', #9424 ) ;
#16711 = PLANE ( 'NONE',  #12040 ) ;
#16712 = CARTESIAN_POINT ( 'NONE',  ( -133.1515905083418545, -69.19806146153663917, 7.897424385335312103 ) ) ;
#16713 = CARTESIAN_POINT ( 'NONE',  ( 133.0181789769776231, -69.32831038615340447, -1.486944123354709824 ) ) ;
#16714 = CARTESIAN_POINT ( 'NONE',  ( -71.18887634719365565, -147.8252249328922687, 49.99999999999999289 ) ) ;
#16715 = DIRECTION ( 'NONE',  ( 1.000000000000000000, 0.000000000000000000, 0.000000000000000000 ) ) ;
#16716 = DIRECTION ( 'NONE',  ( 0.8660254037844363761, 0.5000000000000039968, 0.000000000000000000 ) ) ;
#16717 = ORIENTED_EDGE ( 'NONE', *, *, #16350, .F. ) ;
#16718 = DIRECTION ( 'NONE',  ( 0.000000000000000000, 0.000000000000000000, 1.000000000000000000 ) ) ;
#16719 = ORIENTED_EDGE ( 'NONE', *, *, #9660, .T. ) ;
#16720 = ADVANCED_FACE ( 'NONE', ( #12476 ), #18740, .F. ) ;
#16721 = ORIENTED_EDGE ( 'NONE', *, *, #3510, .T. ) ;
#16722 = VERTEX_POINT ( 'NONE', #17515 ) ;
#16723 = ORIENTED_EDGE ( 'NONE', *, *, #8771, .F. ) ;
#16724 = CARTESIAN_POINT ( 'NONE',  ( -77.21438937758510690, -12.78021302872823384, 248.9926560891072143 ) ) ;
#16725 = CARTESIAN_POINT ( 'NONE',  ( -101.6421356237309226, -200.0000000000000000, 39.99999999999999289 ) ) ;
#16726 = ORIENTED_EDGE ( 'NONE', *, *, #6092, .T. ) ;
#16727 = AXIS2_PLACEMENT_3D ( 'NONE', #642, #10053, #11765 ) ;
#16728 = FACE_OUTER_BOUND ( 'NONE', #4421, .T. ) ;
#16729 = DIRECTION ( 'NONE',  ( -0.000000000000000000, -0.000000000000000000, 1.000000000000000000 ) ) ;
#16730 = EDGE_CURVE ( 'NONE', #1702, #3019, #16565, .T. ) ;
#16731 = ORIENTED_EDGE ( 'NONE', *, *, #1999, .F. ) ;
#16732 = CARTESIAN_POINT ( 'NONE',  ( -100.5012343356710289, 87.83131483863925837, -28.71515701202468662 ) ) ;
#16733 = DIRECTION ( 'NONE',  ( -0.000000000000000000, -0.000000000000000000, 1.000000000000000000 ) ) ;
#16734 = CARTESIAN_POINT ( 'NONE',  ( -2.240720816136038795, 5.281164089014786178, 293.5832628385307999 ) ) ;
#16735 = CARTESIAN_POINT ( 'NONE',  ( -7.500000000000008882, 164.0736214083062805, 49.99999999999999289 ) ) ;
#16736 = CARTESIAN_POINT ( 'NONE',  ( 126.6692879288199833, -80.35371549669886804, 49.11974464924469430 ) ) ;
#16737 = VERTEX_POINT ( 'NONE', #12792 ) ;
#16738 = ADVANCED_FACE ( 'NONE', ( #15669 ), #2062, .F. ) ;
#16739 = DIRECTION ( 'NONE',  ( 0.000000000000000000, 0.000000000000000000, -1.000000000000000000 ) ) ;
#16740 = VECTOR ( 'NONE', #495, 1000.000000000000000 ) ;
#16741 = AXIS2_PLACEMENT_3D ( 'NONE', #13399, #13296, #19650 ) ;
#16742 = ORIENTED_EDGE ( 'NONE', *, *, #2785, .F. ) ;
#16743 = VERTEX_POINT ( 'NONE', #7881 ) ;
#16744 = EDGE_CURVE ( 'NONE', #16612, #5083, #6569, .T. ) ;
#16745 = CARTESIAN_POINT ( 'NONE',  ( -110.0000000000000142, 275.0000000000000000, -94.99999999999997158 ) ) ;
#16746 = ORIENTED_EDGE ( 'NONE', *, *, #8164, .F. ) ;
#16747 = ORIENTED_EDGE ( 'NONE', *, *, #14869, .F. ) ;
#16748 = DIRECTION ( 'NONE',  ( 1.000000000000000000, 0.000000000000000000, 0.000000000000000000 ) ) ;
#16749 = CYLINDRICAL_SURFACE ( 'NONE', #17462, 62.91752772691707207 ) ;
#16750 = DIRECTION ( 'NONE',  ( -1.000000000000000000, 0.000000000000000000, 0.000000000000000000 ) ) ;
#16751 = EDGE_LOOP ( 'NONE', ( #2217, #20151, #3547, #2707 ) ) ;
#16752 = DIRECTION ( 'NONE',  ( 1.000000000000000000, 0.000000000000000000, 0.000000000000000000 ) ) ;
#16753 = DIRECTION ( 'NONE',  ( -0.000000000000000000, -0.000000000000000000, 1.000000000000000000 ) ) ;
#16754 = ORIENTED_EDGE ( 'NONE', *, *, #13456, .F. ) ;
#16755 = ADVANCED_FACE ( 'NONE', ( #14335 ), #5785, .T. ) ;
#16756 = CARTESIAN_POINT ( 'NONE',  ( -127.1451880273208275, -79.59002392720336161, 48.83712415753068825 ) ) ;
#16758 = CIRCLE ( 'NONE', #13151, 112.8770930172170495 ) ;
#16757 = FACE_OUTER_BOUND ( 'NONE', #7921, .T. ) ;
#16759 = AXIS2_PLACEMENT_3D ( 'NONE', #15366, #7800, #17014 ) ;
#16760 = DIRECTION ( 'NONE',  ( -0.000000000000000000, -0.000000000000000000, 1.000000000000000000 ) ) ;
#16761 = EDGE_LOOP ( 'NONE', ( #2368, #7308, #16125, #13822 ) ) ;
#16762 = DIRECTION ( 'NONE',  ( 6.982962677686266711E-15, -0.000000000000000000, 1.000000000000000000 ) ) ;
#16763 = VECTOR ( 'NONE', #5312, 1000.000000000000000 ) ;
#16764 = DIRECTION ( 'NONE',  ( -0.9396926207859105373, 0.3420201433256631063, 0.000000000000000000 ) ) ;
#16765 = CARTESIAN_POINT ( 'NONE',  ( -85.67694800211594952, 110.7245732599958359, 30.17800178787670262 ) ) ;
#16766 = VERTEX_POINT ( 'NONE', #11255 ) ;
#16767 = DIRECTION ( 'NONE',  ( 0.000000000000000000, 0.000000000000000000, -1.000000000000000000 ) ) ;
#16768 = DIRECTION ( 'NONE',  ( -0.000000000000000000, -0.000000000000000000, 1.000000000000000000 ) ) ;
#16769 = CIRCLE ( 'NONE', #11845, 42.50000000000000000 ) ;
#16770 = VERTEX_POINT ( 'NONE', #9821 ) ;
#16771 = EDGE_CURVE ( 'NONE', #4517, #55, #7407, .T. ) ;
#16772 = ORIENTED_EDGE ( 'NONE', *, *, #3621, .F. ) ;
#16773 = ADVANCED_FACE ( 'NONE', ( #12687 ), #14122, .T. ) ;
#16774 = EDGE_CURVE ( 'NONE', #17939, #14181, #1198, .T. ) ;
#16775 = CARTESIAN_POINT ( 'NONE',  ( -83.25760956674176327, -124.7743995867136988, 37.25730000191769165 ) ) ;
#16776 = VECTOR ( 'NONE', #11726, 1000.000000000000227 ) ;
#16777 = ORIENTED_EDGE ( 'NONE', *, *, #13371, .F. ) ;
#16778 = CARTESIAN_POINT ( 'NONE',  ( -50.93469132750304595, -59.42266395395774481, 248.9926560891072143 ) ) ;
#16779 = CARTESIAN_POINT ( 'NONE',  ( 60.00000000000000711, 6.284666409917639535E-13, -105.0000000000000142 ) ) ;
#16780 = VERTEX_POINT ( 'NONE', #1959 ) ;
#16781 = VECTOR ( 'NONE', #16231, 999.9999999999998863 ) ;
#16782 = CARTESIAN_POINT ( 'NONE',  ( 104.7061264979155055, -123.3530444481632742, 0.3798221288333544221 ) ) ;
#16783 = CARTESIAN_POINT ( 'NONE',  ( 159.9599531637113330, -36.50981547336952104, 60.00000000000000000 ) ) ;
#16784 = ADVANCED_FACE ( 'NONE', ( #12888 ), #17314, .T. ) ;
#16785 = AXIS2_PLACEMENT_3D ( 'NONE', #798, #13261, #19523 ) ;
#16786 = PLANE ( 'NONE',  #16677 ) ;
#16787 = LINE ( 'NONE', #7954, #18334 ) ;
#16788 = CARTESIAN_POINT ( 'NONE',  ( -109.9999999999983515, 265.0000000000000000, 92.50000000000004263 ) ) ;
#16789 = DIRECTION ( 'NONE',  ( 1.000000000000000000, 0.000000000000000000, 0.000000000000000000 ) ) ;
#16790 = DIRECTION ( 'NONE',  ( 0.8660254037844397068, -0.4999999999999978906, 0.000000000000000000 ) ) ;
#16791 = CARTESIAN_POINT ( 'NONE',  ( 26.42151830275484770, 4.658826548058130790, 14.88498244535526815 ) ) ;
#16792 = EDGE_LOOP ( 'NONE', ( #4138, #14790, #14107 ) ) ;
#16793 = CARTESIAN_POINT ( 'NONE',  ( -31.77296517111735596, -51.77251465595229263, 293.5832628385307999 ) ) ;
#16794 = CARTESIAN_POINT ( 'NONE',  ( -110.0000000000000142, 275.0000000000000000, -82.50000000000001421 ) ) ;
#16795 = EDGE_CURVE ( 'NONE', #4103, #13430, #2200, .T. ) ;
#16796 = EDGE_LOOP ( 'NONE', ( #15359, #10929, #13970, #5522, #6099 ) ) ;
#16797 = AXIS2_PLACEMENT_3D ( 'NONE', #14246, #15579, #7585 ) ;
#16798 = ORIENTED_EDGE ( 'NONE', *, *, #11418, .T. ) ;
#16799 = MECHANICAL_DESIGN_GEOMETRIC_PRESENTATION_REPRESENTATION (  '', ( #13493 ), #3422 ) ;
#16800 = VERTEX_POINT ( 'NONE', #416 ) ;
#16801 = EDGE_CURVE ( 'NONE', #16155, #3088, #6669, .T. ) ;
#16802 = FACE_BOUND ( 'NONE', #19339, .T. ) ;
#16803 = ORIENTED_EDGE ( 'NONE', *, *, #5616, .F. ) ;
#16804 = LINE ( 'NONE', #6923, #15116 ) ;
#16805 = DIRECTION ( 'NONE',  ( 0.5000000000000044409, 0.8660254037844360431, -4.304393070272782536E-15 ) ) ;
#16806 = DIRECTION ( 'NONE',  ( 1.000000000000000000, 0.000000000000000000, -6.976128451377902853E-15 ) ) ;
#16807 = DIRECTION ( 'NONE',  ( -0.1736481776669241417, -0.9848077530122091305, 0.000000000000000000 ) ) ;
#16808 = CARTESIAN_POINT ( 'NONE',  ( -141.8714406926361562, -48.70825716237266079, 60.00000000000000000 ) ) ;
#16809 = VECTOR ( 'NONE', #6666, 1000.000000000000000 ) ;
#16810 = LINE ( 'NONE', #7805, #9101 ) ;
#16811 = ORIENTED_EDGE ( 'NONE', *, *, #6165, .T. ) ;
#16812 = PLANE ( 'NONE',  #11407 ) ;
#16813 = CARTESIAN_POINT ( 'NONE',  ( -134.6725548700739239, -73.30144156569457436, 8.133873478739229057 ) ) ;
#16814 = CARTESIAN_POINT ( 'NONE',  ( 124.3929425833901803, -83.83509237772305767, -9.887605300484166193 ) ) ;
#16815 = LINE ( 'NONE', #2807, #4966 ) ;
#16816 = CARTESIAN_POINT ( 'NONE',  ( -7.499999999999583444, -60.00000000000000000, -100.0000000000000000 ) ) ;
#16817 = CARTESIAN_POINT ( 'NONE',  ( -134.6061912685141522, -66.19056267105416680, 35.86613249723460228 ) ) ;
#16818 = ORIENTED_EDGE ( 'NONE', *, *, #12878, .T. ) ;
#16819 = CARTESIAN_POINT ( 'NONE',  ( -55.43188410062182925, -19.30071112029661151, 111.4180192758973931 ) ) ;
#16820 = AXIS2_PLACEMENT_3D ( 'NONE', #4999, #8049, #6536 ) ;
#16821 = ORIENTED_EDGE ( 'NONE', *, *, #7233, .F. ) ;
#16822 = AXIS2_PLACEMENT_3D ( 'NONE', #16864, #5929, #10605 ) ;
#16823 = ORIENTED_EDGE ( 'NONE', *, *, #11425, .T. ) ;
#16824 =( BOUNDED_CURVE ( )  B_SPLINE_CURVE ( 3, ( #15199, #19909, #7326, #16949 ),
 .UNSPECIFIED., .F., .F. ) 
 B_SPLINE_CURVE_WITH_KNOTS ( ( 4, 4 ),
 ( 1.570796326794896336, 1.920639998745670596 ),
 .UNSPECIFIED. ) 
 CURVE ( )  GEOMETRIC_REPRESENTATION_ITEM ( )  RATIONAL_B_SPLINE_CURVE ( ( 1.000000000000000000, 0.9898267632596812193, 0.9898267632596812193, 1.000000000000000000 ) ) 
 REPRESENTATION_ITEM ( '' )  );
#16825 = ORIENTED_EDGE ( 'NONE', *, *, #13442, .T. ) ;
#16826 = DIRECTION ( 'NONE',  ( -1.000000000000000000, -0.000000000000000000, -0.000000000000000000 ) ) ;
#16827 = DIRECTION ( 'NONE',  ( -1.000000000000000000, 0.000000000000000000, -0.000000000000000000 ) ) ;
#16828 = DIRECTION ( 'NONE',  ( 0.000000000000000000, -1.000000000000000000, -0.000000000000000000 ) ) ;
#16829 = ORIENTED_EDGE ( 'NONE', *, *, #20100, .F. ) ;
#16831 = CARTESIAN_POINT ( 'NONE',  ( -134.7652707650784407, -31.41120252075685215, -19.73219286542039441 ) ) ;
#16830 = CIRCLE ( 'NONE', #7043, 3.224098631618461663 ) ;
#16832 = CARTESIAN_POINT ( 'NONE',  ( 0.000000000000000000, 0.000000000000000000, 132.4711112102474146 ) ) ;
#16833 = ORIENTED_EDGE ( 'NONE', *, *, #649, .F. ) ;
#16834 = DIRECTION ( 'NONE',  ( 0.000000000000000000, 0.000000000000000000, 1.000000000000000000 ) ) ;
#16835 = DIRECTION ( 'NONE',  ( 0.000000000000000000, 0.000000000000000000, 1.000000000000000000 ) ) ;
#16836 = CARTESIAN_POINT ( 'NONE',  ( 159.9599531637113330, -36.50981547336952104, 49.99999999999999289 ) ) ;
#16837 = FACE_OUTER_BOUND ( 'NONE', #4571, .T. ) ;
#16838 = CARTESIAN_POINT ( 'NONE',  ( 12.14914984460760827, 59.51523122377248853, 293.5832628385307999 ) ) ;
#16839 = CARTESIAN_POINT ( 'NONE',  ( 53.40245231972179596, 28.94983032429848535, 293.5832628385307999 ) ) ;
#16840 = VECTOR ( 'NONE', #3748, 999.9999999999998863 ) ;
#16841 = ORIENTED_EDGE ( 'NONE', *, *, #478, .F. ) ;
#16842 = EDGE_LOOP ( 'NONE', ( #1430, #12143, #9013, #10707 ) ) ;
#16843 = CARTESIAN_POINT ( 'NONE',  ( 113.5802308907675666, 8.308367629983374414, 14.88498244535465709 ) ) ;
#16844 = VERTEX_POINT ( 'NONE', #9623 ) ;
#16845 = MECHANICAL_DESIGN_GEOMETRIC_PRESENTATION_REPRESENTATION (  '', ( #14240 ), #188 ) ;
#16846 = EDGE_LOOP ( 'NONE', ( #10774, #14690, #2999 ) ) ;
#16847 = ADVANCED_FACE ( 'NONE', ( #207 ), #18517, .T. ) ;
#16848 = DIRECTION ( 'NONE',  ( 1.613511099790691498E-16, -1.000000000000000000, -0.000000000000000000 ) ) ;
#16849 = VERTEX_POINT ( 'NONE', #5427 ) ;
#16850 = ORIENTED_EDGE ( 'NONE', *, *, #10904, .F. ) ;
#16851 = LINE ( 'NONE', #7637, #13663 ) ;
#16852 = CARTESIAN_POINT ( 'NONE',  ( -78.68887634719366986, -147.8252249328922687, 39.99999999999999289 ) ) ;
#16853 = CARTESIAN_POINT ( 'NONE',  ( -57.61627707419551570, -19.23614321207253042, 283.5832628385307999 ) ) ;
#16854 = ORIENTED_EDGE ( 'NONE', *, *, #19904, .F. ) ;
#16855 = CARTESIAN_POINT ( 'NONE',  ( -5.524863963826822655, -116.0870680293436408, 14.88498244535549020 ) ) ;
#16856 = CARTESIAN_POINT ( 'NONE',  ( 0.000000000000000000, 0.000000000000000000, 293.5832628385307999 ) ) ;
#16857 = VECTOR ( 'NONE', #9337, 1000.000000000000000 ) ;
#16858 = ORIENTED_EDGE ( 'NONE', *, *, #16862, .T. ) ;
#16859 = EDGE_CURVE ( 'NONE', #98, #19717, #19184, .T. ) ;
#16860 = CARTESIAN_POINT ( 'NONE',  ( 73.61113626724119285, -92.47916748300480094, 14.88498244535493598 ) ) ;
#16861 = CARTESIAN_POINT ( 'NONE',  ( -32.61983739937762294, -51.24071425735592555, 283.5832628385307999 ) ) ;
#16862 = EDGE_CURVE ( 'NONE', #9612, #12285, #4461, .T. ) ;
#16863 = EDGE_CURVE ( 'NONE', #796, #10476, #11336, .T. ) ;
#16864 = CARTESIAN_POINT ( 'NONE',  ( 4.189777606611760026E-13, -60.00000000000000000, -115.0000000000000000 ) ) ;
#16865 = DIRECTION ( 'NONE',  ( -0.000000000000000000, -0.000000000000000000, 1.000000000000000000 ) ) ;
#16866 = CARTESIAN_POINT ( 'NONE',  ( -134.2294018150276429, -76.49442575693799995, 35.55695887397251909 ) ) ;
#16867 = DIRECTION ( 'NONE',  ( 1.000000000000000000, 3.320906611023727849E-16, 0.000000000000000000 ) ) ;
#16868 = ORIENTED_EDGE ( 'NONE', *, *, #16422, .T. ) ;
#16869 = CARTESIAN_POINT ( 'NONE',  ( -71.18887634719365565, -147.8252249328922687, 49.99999999999999289 ) ) ;
#16870 = DIRECTION ( 'NONE',  ( -0.9511061040868804550, -0.3088643371590125697, 0.000000000000000000 ) ) ;
#16871 = ORIENTED_EDGE ( 'NONE', *, *, #8246, .F. ) ;
#16872 = AXIS2_PLACEMENT_3D ( 'NONE', #10603, #9184, #13680 ) ;
#16873 = ORIENTED_EDGE ( 'NONE', *, *, #14144, .F. ) ;
#16874 = EDGE_CURVE ( 'NONE', #1487, #16315, #233, .T. ) ;
#16875 = CARTESIAN_POINT ( 'NONE',  ( -97.21757233051278035, -115.5955488200699932, 29.66285830273704605 ) ) ;
#16876 = AXIS2_PLACEMENT_3D ( 'NONE', #9784, #18135, #15160 ) ;
#16877 = ORIENTED_EDGE ( 'NONE', *, *, #11408, .F. ) ;
#16878 = CARTESIAN_POINT ( 'NONE',  ( 0.000000000000000000, 0.000000000000000000, -105.0000000000000142 ) ) ;
#16879 = VECTOR ( 'NONE', #4459, 1000.000000000000000 ) ;
#16880 = CARTESIAN_POINT ( 'NONE',  ( 7.950000000000000178, 5.196152422706624030, -9.000000000000001776 ) ) ;
#16881 = EDGE_LOOP ( 'NONE', ( #570, #3628, #16653, #3746 ) ) ;
#16882 = CARTESIAN_POINT ( 'NONE',  ( 100.4512631336869504, -129.9078745865736551, 2.904715523906934216 ) ) ;
#16883 = DIRECTION ( 'NONE',  ( 0.000000000000000000, 0.000000000000000000, 1.000000000000000000 ) ) ;
#16884 = EDGE_CURVE ( 'NONE', #9325, #11965, #19628, .T. ) ;
#16885 = CIRCLE ( 'NONE', #6448, 7.500000000000000000 ) ;
#16886 = EDGE_CURVE ( 'NONE', #15284, #18381, #10026, .T. ) ;
#16887 = CARTESIAN_POINT ( 'NONE',  ( -136.7584521108019260, -24.61299102371015479, -18.63592354355825620 ) ) ;
#16888 = DIRECTION ( 'NONE',  ( 1.000000000000000000, 0.000000000000000000, -0.000000000000000000 ) ) ;
#16889 = FACE_BOUND ( 'NONE', #14459, .T. ) ;
#16890 = DIRECTION ( 'NONE',  ( 0.000000000000000000, 0.000000000000000000, 1.000000000000000000 ) ) ;
#16891 = DIRECTION ( 'NONE',  ( 0.000000000000000000, 0.000000000000000000, 1.000000000000000000 ) ) ;
#16892 = CARTESIAN_POINT ( 'NONE',  ( 1.396592535537253342E-14, 0.000000000000000000, 60.00000000000000000 ) ) ;
#16893 = CARTESIAN_POINT ( 'NONE',  ( 96.53160196460632392, -115.8699919790352908, 29.79840038410488745 ) ) ;
#16894 = EDGE_LOOP ( 'NONE', ( #2559, #5190, #6401, #10365 ) ) ;
#16895 = AXIS2_PLACEMENT_3D ( 'NONE', #12275, #12171, #1548 ) ;
#16896 = CARTESIAN_POINT ( 'NONE',  ( -9.176097008934114285, -25.21111933077039069, 14.88498244535551507 ) ) ;
#16897 = LINE ( 'NONE', #9112, #10538 ) ;
#16898 = EDGE_LOOP ( 'NONE', ( #16948, #17855, #11977 ) ) ;
#16899 = ORIENTED_EDGE ( 'NONE', *, *, #7085, .T. ) ;
#16900 = ADVANCED_FACE ( 'NONE', ( #5326 ), #2509, .F. ) ;
#16901 = DIRECTION ( 'NONE',  ( 0.000000000000000000, -1.000000000000000000, 0.000000000000000000 ) ) ;
#16902 = VERTEX_POINT ( 'NONE', #13275 ) ;
#16903 = FACE_BOUND ( 'NONE', #18088, .T. ) ;
#16904 = ORIENTED_EDGE ( 'NONE', *, *, #15739, .F. ) ;
#16905 = CARTESIAN_POINT ( 'NONE',  ( -12.14914984460759761, -59.51523122377249564, 283.5832628385307999 ) ) ;
#16906 = DIRECTION ( 'NONE',  ( -0.000000000000000000, -0.000000000000000000, 1.000000000000000000 ) ) ;
#16907 = VECTOR ( 'NONE', #11708, 1000.000000000000000 ) ;
#16908 = VECTOR ( 'NONE', #16865, 1000.000000000000000 ) ;
#16909 = LINE ( 'NONE', #10447, #9957 ) ;
#16910 = VECTOR ( 'NONE', #17664, 1000.000000000000000 ) ;
#16911 = LINE ( 'NONE', #18140, #11061 ) ;
#16912 = EDGE_CURVE ( 'NONE', #19503, #7379, #19442, .T. ) ;
#16913 = FACE_OUTER_BOUND ( 'NONE', #12836, .T. ) ;
#16914 = EDGE_CURVE ( 'NONE', #16227, #15975, #6956, .T. ) ;
#16915 = ORIENTED_EDGE ( 'NONE', *, *, #12864, .F. ) ;
#16916 = CARTESIAN_POINT ( 'NONE',  ( 73.06915264522001507, 28.06281046684300406, 132.4711112102474146 ) ) ;
#16917 = DIRECTION ( 'NONE',  ( 1.000000000000000000, 0.000000000000000000, 0.000000000000000000 ) ) ;
#16918 = CARTESIAN_POINT ( 'NONE',  ( 131.7304022393856258, -71.85445963696412264, 3.108710632514347871 ) ) ;
#16919 = DIRECTION ( 'NONE',  ( -0.7660444431189749048, -0.6427876096865430267, -0.000000000000000000 ) ) ;
#16920 = CARTESIAN_POINT ( 'NONE',  ( -97.49999999999998579, -133.9542832461881687, 30.00000000000000000 ) ) ;
#16921 = CARTESIAN_POINT ( 'NONE',  ( -133.5298479455752840, -80.72596075552313266, 37.84186899868029741 ) ) ;
#16922 = ADVANCED_FACE ( 'NONE', ( #16571 ), #3782, .T. ) ;
#16923 = VERTEX_POINT ( 'NONE', #19534 ) ;
#16924 = DIRECTION ( 'NONE',  ( -0.000000000000000000, -0.000000000000000000, 1.000000000000000000 ) ) ;
#16925 = AXIS2_PLACEMENT_3D ( 'NONE', #4872, #6204, #14375 ) ;
#16926 = AXIS2_PLACEMENT_3D ( 'NONE', #17567, #14851, #13302 ) ;
#16927 = ORIENTED_EDGE ( 'NONE', *, *, #15735, .F. ) ;
#16928 = ORIENTED_EDGE ( 'NONE', *, *, #15530, .F. ) ;
#16929 = ORIENTED_EDGE ( 'NONE', *, *, #10969, .T. ) ;
#16930 = CARTESIAN_POINT ( 'NONE',  ( -141.7593571144487044, -18.51227725722888096, 19.71492705251383981 ) ) ;
#16931 = FACE_OUTER_BOUND ( 'NONE', #3527, .T. ) ;
#16932 = CARTESIAN_POINT ( 'NONE',  ( 0.000000000000000000, 0.000000000000000000, 248.9926560891072143 ) ) ;
#16933 = VERTEX_POINT ( 'NONE', #17811 ) ;
#16934 = VECTOR ( 'NONE', #13259, 1000.000000000000114 ) ;
#16935 = DIRECTION ( 'NONE',  ( -0.000000000000000000, -0.000000000000000000, 1.000000000000000000 ) ) ;
#16936 = DIRECTION ( 'NONE',  ( -0.7660444431189725734, -0.6427876096865456912, 0.000000000000000000 ) ) ;
#16937 = VECTOR ( 'NONE', #5270, 1000.000000000000114 ) ;
#16938 = VERTEX_POINT ( 'NONE', #17909 ) ;
#16939 = CARTESIAN_POINT ( 'NONE',  ( -91.39357229321551301, 100.9612215610973038, -24.64723702058964605 ) ) ;
#16940 = AXIS2_PLACEMENT_3D ( 'NONE', #3786, #10032, #16480 ) ;
#16941 = LINE ( 'NONE', #12115, #12633 ) ;
#16942 = CYLINDRICAL_SURFACE ( 'NONE', #15000, 150.0000000000000284 ) ;
#16943 = CYLINDRICAL_SURFACE ( 'NONE', #993, 62.91752772691707207 ) ;
#16944 = CARTESIAN_POINT ( 'NONE',  ( -45.84586732611835913, 36.66871011346426457, 110.7293897666001214 ) ) ;
#16945 = LINE ( 'NONE', #18173, #16588 ) ;
#16946 = CARTESIAN_POINT ( 'NONE',  ( 0.000000000000000000, 0.000000000000000000, 293.5832628385307999 ) ) ;
#16947 = ORIENTED_EDGE ( 'NONE', *, *, #4419, .F. ) ;
#16948 = ORIENTED_EDGE ( 'NONE', *, *, #457, .F. ) ;
#16949 = CARTESIAN_POINT ( 'NONE',  ( -176.7850001792984926, -190.0000000000000284, 33.42750952962406075 ) ) ;
#16950 = ORIENTED_EDGE ( 'NONE', *, *, #6295, .F. ) ;
#16951 = AXIS2_PLACEMENT_3D ( 'NONE', #18712, #4800, #6335 ) ;
#16952 = AXIS2_PLACEMENT_3D ( 'NONE', #13373, #15215, #12036 ) ;
#16953 = ORIENTED_EDGE ( 'NONE', *, *, #1642, .F. ) ;
#16954 = DIRECTION ( 'NONE',  ( 0.000000000000000000, 0.000000000000000000, -1.000000000000000000 ) ) ;
#16955 = CIRCLE ( 'NONE', #14974, 150.0000000000000284 ) ;
#16956 = VERTEX_POINT ( 'NONE', #14727 ) ;
#16957 = LINE ( 'NONE', #2946, #12941 ) ;
#16958 = CARTESIAN_POINT ( 'NONE',  ( 0.1469846612282419140, -6.696526368584444278, 6.401276095387000709 ) ) ;
#16959 = CARTESIAN_POINT ( 'NONE',  ( -32.61983739937760873, -51.24071425735591134, 293.5832628385307999 ) ) ;
#16960 = CARTESIAN_POINT ( 'NONE',  ( -110.0000000000000142, 285.0000000000000568, -75.00000000000000000 ) ) ;
#16961 = VERTEX_POINT ( 'NONE', #7163 ) ;
#16962 = CARTESIAN_POINT ( 'NONE',  ( 0.09252763182291959265, 6.914127053141843504, -6.024380653971843635 ) ) ;
#16963 = LINE ( 'NONE', #10709, #3245 ) ;
#16964 = ORIENTED_EDGE ( 'NONE', *, *, #2727, .F. ) ;
#16965 = CARTESIAN_POINT ( 'NONE',  ( -127.4413876050234933, 1.560706874093891806E-14, 39.88498244535634285 ) ) ;
#16966 = DIRECTION ( 'NONE',  ( 1.000000000000000000, 0.000000000000000000, 0.000000000000000000 ) ) ;
#16967 = VECTOR ( 'NONE', #17010, 1000.000000000000227 ) ;
#16968 = CIRCLE ( 'NONE', #4543, 150.0000000000000284 ) ;
#16969 = ADVANCED_FACE ( 'NONE', ( #16276 ), #5620, .T. ) ;
#16970 = CARTESIAN_POINT ( 'NONE',  ( 0.000000000000000000, 0.000000000000000000, 248.9926560891072143 ) ) ;
#16971 = DIRECTION ( 'NONE',  ( 1.000000000000000000, 0.000000000000000000, 0.000000000000000000 ) ) ;
#16972 = CARTESIAN_POINT ( 'NONE',  ( 7.350000000000000533, -5.196152422706636465, -8.999999999999998224 ) ) ;
#16973 = DIRECTION ( 'NONE',  ( -6.982962677686266711E-15, 0.000000000000000000, -1.000000000000000000 ) ) ;
#16974 = VERTEX_POINT ( 'NONE', #713 ) ;
#16975 = DIRECTION ( 'NONE',  ( 1.000000000000000000, 0.000000000000000000, 0.000000000000000000 ) ) ;
#16976 = FACE_OUTER_BOUND ( 'NONE', #1014, .T. ) ;
#16977 = ORIENTED_EDGE ( 'NONE', *, *, #3856, .F. ) ;
#16978 = VERTEX_POINT ( 'NONE', #7060 ) ;
#16979 = CARTESIAN_POINT ( 'NONE',  ( 0.000000000000000000, 0.000000000000000000, 293.5832628385307999 ) ) ;
#16980 = EDGE_CURVE ( 'NONE', #9322, #16974, #16475, .T. ) ;
#16981 = ORIENTED_EDGE ( 'NONE', *, *, #5577, .T. ) ;
#16982 = VECTOR ( 'NONE', #11545, 1000.000000000000114 ) ;
#16983 = AXIS2_PLACEMENT_3D ( 'NONE', #6509, #13029, #19089 ) ;
#16984 = EDGE_CURVE ( 'NONE', #15949, #10094, #13177, .T. ) ;
#16985 = CARTESIAN_POINT ( 'NONE',  ( -109.9999999999983515, 265.0000000000000000, 85.00000000000001421 ) ) ;
#16986 = CARTESIAN_POINT ( 'NONE',  ( 0.000000000000000000, 0.000000000000000000, 248.9926560891072143 ) ) ;
#16987 = VERTEX_POINT ( 'NONE', #2550 ) ;
#16988 = CARTESIAN_POINT ( 'NONE',  ( 97.58310720701103946, -133.8455726501578908, 8.700002021410107034 ) ) ;
#16989 = DIRECTION ( 'NONE',  ( 0.000000000000000000, 0.000000000000000000, 1.000000000000000000 ) ) ;
#16990 = ADVANCED_FACE ( 'NONE', ( #2452 ), #14630, .T. ) ;
#16991 = CARTESIAN_POINT ( 'NONE',  ( -135.7615415765321814, -31.23721399736636428, -16.61340895829727060 ) ) ;
#16992 = DIRECTION ( 'NONE',  ( -0.9396926207859115365, 0.3420201433256602197, 0.000000000000000000 ) ) ;
#16993 = CARTESIAN_POINT ( 'NONE',  ( 51.24071425735603214, -32.61983739937743110, 283.5832628385307999 ) ) ;
#16994 = ORIENTED_EDGE ( 'NONE', *, *, #1880, .T. ) ;
#16995 = LINE ( 'NONE', #2982, #2385 ) ;
#16996 = AXIS2_PLACEMENT_3D ( 'NONE', #13298, #7275, #2476 ) ;
#16997 = CARTESIAN_POINT ( 'NONE',  ( -20.74471755083564162, 59.39925916207566559, 132.4711112102474146 ) ) ;
#16998 = DIRECTION ( 'NONE',  ( 0.000000000000000000, 0.000000000000000000, 1.000000000000000000 ) ) ;
#16999 = CIRCLE ( 'NONE', #14713, 106.4288957539801004 ) ;
#17000 = CARTESIAN_POINT ( 'NONE',  ( 99.35657680079279430, -131.4542451999401749, 35.80648205613542956 ) ) ;
#17001 = ORIENTED_EDGE ( 'NONE', *, *, #17056, .F. ) ;
#17002 = FACE_OUTER_BOUND ( 'NONE', #15978, .T. ) ;
#17003 = DIRECTION ( 'NONE',  ( -0.000000000000000000, -0.000000000000000000, 1.000000000000000000 ) ) ;
#17004 = ORIENTED_EDGE ( 'NONE', *, *, #10582, .T. ) ;
#17005 = ORIENTED_EDGE ( 'NONE', *, *, #14879, .T. ) ;
#17006 = EDGE_CURVE ( 'NONE', #383, #9853, #5146, .T. ) ;
#17007 = ADVANCED_FACE ( 'NONE', ( #19725 ), #7652, .T. ) ;
#17008 = EDGE_LOOP ( 'NONE', ( #15751, #13793, #1638, #8423 ) ) ;
#17009 = ADVANCED_FACE ( 'NONE', ( #6033 ), #7549, .F. ) ;
#17010 = DIRECTION ( 'NONE',  ( -0.8479630283625716469, 0.5300553768524345344, 0.000000000000000000 ) ) ;
#17011 = PLANE ( 'NONE',  #6751 ) ;
#17012 = ORIENTED_EDGE ( 'NONE', *, *, #5556, .T. ) ;
#17013 = VECTOR ( 'NONE', #1743, 1000.000000000000000 ) ;
#17014 = DIRECTION ( 'NONE',  ( -0.8660254037844397068, 0.4999999999999978906, 0.000000000000000000 ) ) ;
#17015 = CARTESIAN_POINT ( 'NONE',  ( 166.7850001792985495, -199.9999999999999716, 40.00000000000000000 ) ) ;
#17016 = CARTESIAN_POINT ( 'NONE',  ( -2.240720816136042348, 5.281164089014786178, 293.5832628385307999 ) ) ;
#17017 = CARTESIAN_POINT ( 'NONE',  ( -100.4512631336862825, -129.9078745865736551, 37.09528447609245916 ) ) ;
#17018 = CARTESIAN_POINT ( 'NONE',  ( 76.92888220842486646, -14.39940464655733976, 112.0427633081292385 ) ) ;
#17019 = DIRECTION ( 'NONE',  ( -6.982962677686266711E-15, 0.000000000000000000, -1.000000000000000000 ) ) ;
#17020 = CARTESIAN_POINT ( 'NONE',  ( 0.000000000000000000, 0.000000000000000000, 283.5832628385307999 ) ) ;
#17021 = CARTESIAN_POINT ( 'NONE',  ( -133.9967726966432053, -77.99266392030686745, 3.479247166016994353 ) ) ;
#17022 = ADVANCED_FACE ( 'NONE', ( #19928 ), #7252, .T. ) ;
#17023 = CARTESIAN_POINT ( 'NONE',  ( 128.4532923017994506, -77.52586173742918163, -0.4241867359497863976 ) ) ;
#17024 = LINE ( 'NONE', #9343, #12442 ) ;
#17025 = DIRECTION ( 'NONE',  ( 6.982962677686266711E-15, -0.000000000000000000, 1.000000000000000000 ) ) ;
#17026 = CARTESIAN_POINT ( 'NONE',  ( -125.0010599886705620, -82.93257931481025480, 40.94260748306679432 ) ) ;
#17027 = ORIENTED_EDGE ( 'NONE', *, *, #13878, .T. ) ;
#17028 = VECTOR ( 'NONE', #60, 1000.000000000000000 ) ;
#17029 = DIRECTION ( 'NONE',  ( -1.000000000000000000, 0.000000000000000000, 0.000000000000000000 ) ) ;
#17030 = VECTOR ( 'NONE', #40, 1000.000000000000114 ) ;
#17031 = ORIENTED_EDGE ( 'NONE', *, *, #7063, .T. ) ;
#17032 = EDGE_CURVE ( 'NONE', #18743, #20112, #1888, .T. ) ;
#17033 = EDGE_CURVE ( 'NONE', #6781, #12002, #15432, .T. ) ;
#17034 = VERTEX_POINT ( 'NONE', #8978 ) ;
#17035 = EDGE_CURVE ( 'NONE', #2271, #12416, #13474, .T. ) ;
#17036 = VECTOR ( 'NONE', #15897, 1000.000000000000000 ) ;
#17037 = VERTEX_POINT ( 'NONE', #17074 ) ;
#17038 = CARTESIAN_POINT ( 'NONE',  ( -9.544791666812290742, 100.7028639675991855, 14.88498244535551862 ) ) ;
#17039 = VECTOR ( 'NONE', #5950, 1000.000000000000114 ) ;
#17040 = CARTESIAN_POINT ( 'NONE',  ( -53.78543575132151489, -32.64570716507521553, 293.5832628385307999 ) ) ;
#17041 = CARTESIAN_POINT ( 'NONE',  ( 163.5019688434126977, -20.99123081650019884, 49.99999999999999289 ) ) ;
#17042 = ORIENTED_EDGE ( 'NONE', *, *, #13129, .T. ) ;
#17043 = DIRECTION ( 'NONE',  ( 0.000000000000000000, 0.000000000000000000, -1.000000000000000000 ) ) ;
#17044 = DIRECTION ( 'NONE',  ( 6.982962677686266711E-15, -0.000000000000000000, 1.000000000000000000 ) ) ;
#17045 = ORIENTED_EDGE ( 'NONE', *, *, #15013, .F. ) ;
#17046 = CARTESIAN_POINT ( 'NONE',  ( -90.37486697571327454, 102.3558818120413321, -23.98309657527855165 ) ) ;
#17047 = DIRECTION ( 'NONE',  ( -0.7881095627315619634, -0.6155349844899687950, 0.000000000000000000 ) ) ;
#17048 = DIRECTION ( 'NONE',  ( 1.000000000000000000, 0.000000000000000000, 0.000000000000000000 ) ) ;
#17049 = DIRECTION ( 'NONE',  ( 0.000000000000000000, 0.000000000000000000, -1.000000000000000000 ) ) ;
#17050 = DIRECTION ( 'NONE',  ( 0.000000000000000000, 0.000000000000000000, 1.000000000000000000 ) ) ;
#17051 = CARTESIAN_POINT ( 'NONE',  ( 131.8415137303879874, -71.65490762087030419, 36.74244028875413193 ) ) ;
#17052 = FACE_OUTER_BOUND ( 'NONE', #17574, .T. ) ;
#17053 = ORIENTED_EDGE ( 'NONE', *, *, #20100, .T. ) ;
#17054 = VERTEX_POINT ( 'NONE', #13891 ) ;
#17055 = ORIENTED_EDGE ( 'NONE', *, *, #13494, .T. ) ;
#17056 = EDGE_CURVE ( 'NONE', #15465, #1187, #5160, .T. ) ;
#17057 = ORIENTED_EDGE ( 'NONE', *, *, #5782, .T. ) ;
#17058 = CARTESIAN_POINT ( 'NONE',  ( 0.000000000000000000, 60.00000000000000000, -115.0000000000000000 ) ) ;
#17059 = VECTOR ( 'NONE', #6691, 999.9999999999998863 ) ;
#17060 = ORIENTED_EDGE ( 'NONE', *, *, #13642, .F. ) ;
#17061 = DIRECTION ( 'NONE',  ( 1.000000000000000000, 0.000000000000000000, -6.994638739193269649E-15 ) ) ;
#17062 = EDGE_CURVE ( 'NONE', #3790, #7238, #6133, .T. ) ;
#17063 = CARTESIAN_POINT ( 'NONE',  ( 0.000000000000000000, -7.794228634059936489, 4.500000000000017764 ) ) ;
#17064 = SURFACE_STYLE_FILL_AREA ( #13674 ) ;
#17065 = CARTESIAN_POINT ( 'NONE',  ( -103.8888757476053541, -46.65403860089418941, 14.88498244535617765 ) ) ;
#17066 = ORIENTED_EDGE ( 'NONE', *, *, #2526, .T. ) ;
#17067 = FACE_OUTER_BOUND ( 'NONE', #9632, .T. ) ;
#17068 = DIRECTION ( 'NONE',  ( 0.000000000000000000, 1.000000000000000000, 0.000000000000000000 ) ) ;
#17069 = ORIENTED_EDGE ( 'NONE', *, *, #20144, .F. ) ;
#17070 = CARTESIAN_POINT ( 'NONE',  ( -60.00000000000000000, -2.094888803305880013E-13, -105.0000000000000142 ) ) ;
#17071 = DIRECTION ( 'NONE',  ( 0.000000000000000000, 0.000000000000000000, 1.000000000000000000 ) ) ;
#17072 = DIRECTION ( 'NONE',  ( 0.3420201433256757073, -0.9396926207859057634, 0.000000000000000000 ) ) ;
#17073 = AXIS2_PLACEMENT_3D ( 'NONE', #17884, #7303, #16718 ) ;
#17074 = CARTESIAN_POINT ( 'NONE',  ( 7.350000000000000533, 10.39230484541327471, 0.000000000000000000 ) ) ;
#17075 = FACE_OUTER_BOUND ( 'NONE', #866, .T. ) ;
#17076 = CARTESIAN_POINT ( 'NONE',  ( -77.41967535438791970, 116.6460954727662767, 17.81468430219124244 ) ) ;
#17077 = ORIENTED_EDGE ( 'NONE', *, *, #17417, .F. ) ;
#17078 = CARTESIAN_POINT ( 'NONE',  ( 148.9554720520395108, -17.67108784863215476, 39.99999999999999289 ) ) ;
#17079 = ORIENTED_EDGE ( 'NONE', *, *, #5251, .F. ) ;
#17080 = AXIS2_PLACEMENT_3D ( 'NONE', #5622, #10312, #2552 ) ;
#17081 = ORIENTED_EDGE ( 'NONE', *, *, #2609, .T. ) ;
#17082 = CARTESIAN_POINT ( 'NONE',  ( 57.61627707419550148, 19.23614321207255529, 283.5832628385307999 ) ) ;
#17083 = EDGE_LOOP ( 'NONE', ( #3644, #19836, #4902, #15289 ) ) ;
#17084 = EDGE_CURVE ( 'NONE', #6026, #1034, #15025, .T. ) ;
#17085 = DIRECTION ( 'NONE',  ( -1.000000000000000000, 0.000000000000000000, 0.000000000000000000 ) ) ;
#17086 = CARTESIAN_POINT ( 'NONE',  ( 0.000000000000000000, 0.000000000000000000, 293.5832628385307999 ) ) ;
#17087 = VECTOR ( 'NONE', #10537, 1000.000000000000000 ) ;
#17088 = EDGE_LOOP ( 'NONE', ( #4165, #875, #12011, #17323, #15501, #3834 ) ) ;
#17089 = CARTESIAN_POINT ( 'NONE',  ( 82.80829968034944955, -125.0716697069634336, 4.111516946209861523 ) ) ;
#17090 = CARTESIAN_POINT ( 'NONE',  ( 0.000000000000000000, 0.000000000000000000, 283.5832628385307999 ) ) ;
#17091 = DIRECTION ( 'NONE',  ( -0.000000000000000000, -0.000000000000000000, 1.000000000000000000 ) ) ;
#17092 = CARTESIAN_POINT ( 'NONE',  ( -115.2828271789294803, -14.71737894807794156, 39.88498244535625759 ) ) ;
#17093 = ORIENTED_EDGE ( 'NONE', *, *, #6909, .F. ) ;
#17094 = EDGE_CURVE ( 'NONE', #1901, #6781, #12146, .T. ) ;
#17095 = DIRECTION ( 'NONE',  ( 0.000000000000000000, 0.000000000000000000, -1.000000000000000000 ) ) ;
#17096 = DIRECTION ( 'NONE',  ( -0.000000000000000000, -0.000000000000000000, 1.000000000000000000 ) ) ;
#17097 = CARTESIAN_POINT ( 'NONE',  ( 25.99419088092191643, -73.82206860051539365, 111.4180192758973362 ) ) ;
#17098 = CARTESIAN_POINT ( 'NONE',  ( 97.50000000000001421, -133.9542832461881687, 30.00000000000000000 ) ) ;
#17099 = ORIENTED_EDGE ( 'NONE', *, *, #13003, .T. ) ;
#17100 = FACE_OUTER_BOUND ( 'NONE', #15983, .T. ) ;
#17101 = CARTESIAN_POINT ( 'NONE',  ( 40.28046525994349736, 45.46865632508086463, 283.5832628385307999 ) ) ;
#17102 = VECTOR ( 'NONE', #13063, 1000.000000000000114 ) ;
#17103 = ORIENTED_EDGE ( 'NONE', *, *, #19389, .F. ) ;
#17104 = VERTEX_POINT ( 'NONE', #1316 ) ;
#17105 = ORIENTED_EDGE ( 'NONE', *, *, #896, .T. ) ;
#17106 = CARTESIAN_POINT ( 'NONE',  ( 0.000000000000000000, 0.000000000000000000, 0.000000000000000000 ) ) ;
#17107 = CIRCLE ( 'NONE', #16797, 27.50000000000000355 ) ;
#17108 = ORIENTED_EDGE ( 'NONE', *, *, #16886, .T. ) ;
#17109 = EDGE_CURVE ( 'NONE', #12789, #13695, #15219, .T. ) ;
#17110 = CARTESIAN_POINT ( 'NONE',  ( 141.8871031824808995, -16.05777877957299538, 39.99999999999999289 ) ) ;
#17111 = EDGE_CURVE ( 'NONE', #1300, #18061, #4153, .T. ) ;
#17112 = DIRECTION ( 'NONE',  ( 0.000000000000000000, 0.000000000000000000, -1.000000000000000000 ) ) ;
#17113 = MECHANICAL_DESIGN_GEOMETRIC_PRESENTATION_REPRESENTATION (  '', ( #5053 ), #3069 ) ;
#17114 = ORIENTED_EDGE ( 'NONE', *, *, #18155, .F. ) ;
#17115 = CARTESIAN_POINT ( 'NONE',  ( 7.350000000000000533, -10.39230484541326582, 0.000000000000000000 ) ) ;
#17116 = DIRECTION ( 'NONE',  ( -0.6155349844899689060, 0.7881095627315620744, 0.000000000000000000 ) ) ;
#17117 = CARTESIAN_POINT ( 'NONE',  ( 133.3415482518558406, -68.70949856429523095, 40.71953839863250124 ) ) ;
#17118 = CARTESIAN_POINT ( 'NONE',  ( -95.45795901651536042, -116.1130648478386291, 32.13249062836397485 ) ) ;
#17119 = CARTESIAN_POINT ( 'NONE',  ( -167.4599531637108782, -36.50981547337168109, 39.99999999999999289 ) ) ;
#17120 = DIRECTION ( 'NONE',  ( -0.000000000000000000, -0.000000000000000000, 1.000000000000000000 ) ) ;
#17121 = CARTESIAN_POINT ( 'NONE',  ( 11.00103590902871353, 57.65577537092163851, 248.9926560891072143 ) ) ;
#17122 = FACE_OUTER_BOUND ( 'NONE', #19584, .T. ) ;
#17123 = EDGE_CURVE ( 'NONE', #2635, #7392, #15120, .T. ) ;
#17124 = CARTESIAN_POINT ( 'NONE',  ( 132.9666886943622330, -83.66363014848037949, 1.140117263048182616 ) ) ;
#17125 = EDGE_CURVE ( 'NONE', #9946, #6087, #248, .T. ) ;
#17126 = CIRCLE ( 'NONE', #8618, 17.50000000000000355 ) ;
#17127 = LINE ( 'NONE', #14051, #17030 ) ;
#17128 = CARTESIAN_POINT ( 'NONE',  ( 48.89172014028660129, 94.20918150411493741, 14.88498244535511184 ) ) ;
#17129 = CARTESIAN_POINT ( 'NONE',  ( -133.6471402512195539, -68.10643054410131469, 39.75618603187317035 ) ) ;
#17130 = ORIENTED_EDGE ( 'NONE', *, *, #11590, .F. ) ;
#17131 = ADVANCED_FACE ( 'NONE', ( #13789 ), #18303, .T. ) ;
#17132 = DIRECTION ( 'NONE',  ( -0.000000000000000000, 0.000000000000000000, -1.000000000000000000 ) ) ;
#17133 = VECTOR ( 'NONE', #4764, 1000.000000000000114 ) ;
#17134 = ORIENTED_EDGE ( 'NONE', *, *, #8028, .F. ) ;
#17135 = ORIENTED_EDGE ( 'NONE', *, *, #13640, .F. ) ;
#17136 = EDGE_CURVE ( 'NONE', #9872, #9804, #5932, .T. ) ;
#17137 = EDGE_CURVE ( 'NONE', #7108, #15648, #7423, .T. ) ;
#17138 = ORIENTED_EDGE ( 'NONE', *, *, #15385, .F. ) ;
#17139 = VECTOR ( 'NONE', #2473, 1000.000000000000000 ) ;
#17140 = CARTESIAN_POINT ( 'NONE',  ( -145.0046799159938473, -14.11398466591643341, 5.837281836175630900 ) ) ;
#17141 = CARTESIAN_POINT ( 'NONE',  ( 28.94886449118905247, -53.40063514825087054, 293.5832628385307999 ) ) ;
#17142 = CIRCLE ( 'NONE', #8317, 7.500000000000020428 ) ;
#17143 = DIRECTION ( 'NONE',  ( -0.3088643371590125697, 0.9511061040868803440, 0.000000000000000000 ) ) ;
#17144 = ORIENTED_EDGE ( 'NONE', *, *, #11490, .F. ) ;
#17145 = CARTESIAN_POINT ( 'NONE',  ( 59.51724408343574879, -12.14957802882732452, 283.5832628385307999 ) ) ;
#17146 = LINE ( 'NONE', #8225, #1627 ) ;
#17147 = CARTESIAN_POINT ( 'NONE',  ( -90.03415420018352222, 102.8177110809194801, -23.74958468013522506 ) ) ;
#17148 = DIRECTION ( 'NONE',  ( 1.000000000000000000, 0.000000000000000000, 0.000000000000000000 ) ) ;
#17149 = DIRECTION ( 'NONE',  ( 6.982962677686266711E-15, -0.000000000000000000, 1.000000000000000000 ) ) ;
#17150 = EDGE_CURVE ( 'NONE', #6726, #2555, #7111, .T. ) ;
#17151 = CARTESIAN_POINT ( 'NONE',  ( 3.304959094393253416, 31.03941509555038181, 14.88498244535543158 ) ) ;
#17152 = VECTOR ( 'NONE', #4092, 1000.000000000000000 ) ;
#17153 = LINE ( 'NONE', #1392, #2216 ) ;
#17154 = ADVANCED_FACE ( 'NONE', ( #1826 ), #6239, .F. ) ;
#17155 = PRODUCT_DEFINITION ( 'UNKNOWN', '', #8512, #10076 ) ;
#17156 = EDGE_CURVE ( 'NONE', #11965, #20114, #6641, .T. ) ;
#17157 = CARTESIAN_POINT ( 'NONE',  ( 130.7712900376312462, -73.57687123476455326, 38.42272532816287622 ) ) ;
#17158 = VECTOR ( 'NONE', #4697, 1000.000000000000000 ) ;
#17159 = LINE ( 'NONE', #4779, #854 ) ;
#17160 = ORIENTED_EDGE ( 'NONE', *, *, #237, .T. ) ;
#17161 = ORIENTED_EDGE ( 'NONE', *, *, #17035, .F. ) ;
#17162 = ORIENTED_EDGE ( 'NONE', *, *, #9627, .T. ) ;
#17163 = VERTEX_POINT ( 'NONE', #17183 ) ;
#17164 = CARTESIAN_POINT ( 'NONE',  ( 148.9554720520395392, -17.67108784863215831, 49.99999999999999289 ) ) ;
#17165 = EDGE_CURVE ( 'NONE', #7250, #2555, #14408, .T. ) ;
#17166 = ORIENTED_EDGE ( 'NONE', *, *, #18630, .F. ) ;
#17167 = PLANE ( 'NONE',  #8375 ) ;
#17168 = AXIS2_PLACEMENT_3D ( 'NONE', #16465, #4067, #2648 ) ;
#17169 = CARTESIAN_POINT ( 'NONE',  ( 51.36153797460909232, -59.06449708980179736, 132.4711112102474146 ) ) ;
#17170 = CARTESIAN_POINT ( 'NONE',  ( 60.72073886220397299, -1.629865514042299512, 293.5832628385307999 ) ) ;
#17171 = CARTESIAN_POINT ( 'NONE',  ( -29.99999999999887379, 285.0000000000000568, -2.500000000000847766 ) ) ;
#17172 = LINE ( 'NONE', #280, #14303 ) ;
#17173 = ORIENTED_EDGE ( 'NONE', *, *, #19019, .F. ) ;
#17174 = CARTESIAN_POINT ( 'NONE',  ( 0.000000000000000000, 0.000000000000000000, 248.9926560891072143 ) ) ;
#17175 = CARTESIAN_POINT ( 'NONE',  ( 67.50000000000000000, 6.284666409917639535E-13, -105.0000000000000142 ) ) ;
#17176 = EDGE_LOOP ( 'NONE', ( #16574, #11139, #14403, #1530 ) ) ;
#17177 = B_SPLINE_CURVE_WITH_KNOTS ( 'NONE', 3,
 ( #18814, #5100, #12952, #180, #15937, #19211, #14499, #1925, #3257, #14400, #11218, #5201, #11015, #3454, #17582, #12758, #4903, #381, #8351, #8251, #11430, #6633, #484, #11326, #12857, #17481 ),
 .UNSPECIFIED., .F., .F.,
 ( 4, 2, 2, 2, 2, 2, 2, 2, 2, 2, 2, 2, 4 ),
 ( 0.000000000000000000, 0.004334419010350961353, 0.006501628515526464147, 0.008668838020701969543, 0.01300325703105293350, 0.01517046653622841808, 0.01733767604140390439, 0.02167209505175490478, 0.02383930455693041364, 0.02600651406210592251, 0.02817372356728143831, 0.03034093307245694718, 0.03467535208280797532 ),
 .UNSPECIFIED. ) ;
#17178 = DIRECTION ( 'NONE',  ( 0.7818314824680226982, 0.6234898018587423651, 0.000000000000000000 ) ) ;
#17179 = FACE_OUTER_BOUND ( 'NONE', #8775, .T. ) ;
#17180 = EDGE_CURVE ( 'NONE', #2426, #2170, #11337, .T. ) ;
#17181 = EDGE_CURVE ( 'NONE', #5705, #5779, #12766, .T. ) ;
#17182 = LINE ( 'NONE', #3164, #11592 ) ;
#17183 = CARTESIAN_POINT ( 'NONE',  ( 141.8714406926368099, -48.70825716237082759, 60.00000000000000000 ) ) ;
#17184 = LINE ( 'NONE', #12455, #8816 ) ;
#17185 = CARTESIAN_POINT ( 'NONE',  ( -68.18670162478831287, -38.41834839689355618, 132.4711112102474146 ) ) ;
#17186 = EDGE_CURVE ( 'NONE', #675, #244, #11348, .T. ) ;
#17187 = ORIENTED_EDGE ( 'NONE', *, *, #11246, .F. ) ;
#17188 = FACE_OUTER_BOUND ( 'NONE', #552, .T. ) ;
#17189 = ORIENTED_EDGE ( 'NONE', *, *, #9175, .T. ) ;
#17190 = APPLICATION_CONTEXT ( 'automotive_design' ) ;
#17191 = VERTEX_POINT ( 'NONE', #1524 ) ;
#17192 = CARTESIAN_POINT ( 'NONE',  ( 82.03125000000004263, -125.5821405433013638, 49.99999999999999289 ) ) ;
#17193 = ORIENTED_EDGE ( 'NONE', *, *, #11104, .T. ) ;
#17194 = AXIS2_PLACEMENT_3D ( 'NONE', #17873, #19593, #778 ) ;
#17195 = CARTESIAN_POINT ( 'NONE',  ( 0.000000000000000000, 0.000000000000000000, 248.9926560891072143 ) ) ;
#17196 = DIRECTION ( 'NONE',  ( -0.000000000000000000, -0.000000000000000000, 1.000000000000000000 ) ) ;
#17197 = ORIENTED_EDGE ( 'NONE', *, *, #7004, .T. ) ;
#17198 = CARTESIAN_POINT ( 'NONE',  ( 56.50329132715945235, -22.30005961346246579, 283.5832628385307999 ) ) ;
#17199 = PLANE ( 'NONE',  #4785 ) ;
#17200 = CIRCLE ( 'NONE', #3146, 7.500000000000020428 ) ;
#17201 = CARTESIAN_POINT ( 'NONE',  ( 48.17959877923549072, 36.99514631729036296, 293.5832628385307999 ) ) ;
#17202 = DIRECTION ( 'NONE',  ( -0.1736481776669409338, -0.9848077530122062440, 2.152196535136391268E-15 ) ) ;
#17203 = ORIENTED_EDGE ( 'NONE', *, *, #14284, .T. ) ;
#17204 = CARTESIAN_POINT ( 'NONE',  ( -12.28122767885803945, 61.70726652483829611, 132.4711112102474146 ) ) ;
#17205 = CARTESIAN_POINT ( 'NONE',  ( -159.9599531637108782, -36.50981547337168109, 49.99999999999999289 ) ) ;
#17206 = DIRECTION ( 'NONE',  ( 0.000000000000000000, 0.000000000000000000, 1.000000000000000000 ) ) ;
#17207 = CARTESIAN_POINT ( 'NONE',  ( -73.82206860051549313, -25.99419088092168195, 132.4711112102474146 ) ) ;
#17208 = CIRCLE ( 'NONE', #14251, 106.4288957539801004 ) ;
#17209 = ORIENTED_EDGE ( 'NONE', *, *, #13900, .T. ) ;
#17210 = AXIS2_PLACEMENT_3D ( 'NONE', #19762, #10252, #1142 ) ;
#17211 = LINE ( 'NONE', #9111, #15614 ) ;
#17212 = DIRECTION ( 'NONE',  ( 1.000000000000000000, -2.775557561562892929E-15, 0.000000000000000000 ) ) ;
#17213 = ORIENTED_EDGE ( 'NONE', *, *, #13864, .T. ) ;
#17214 = ORIENTED_EDGE ( 'NONE', *, *, #18673, .T. ) ;
#17216 = ORIENTED_EDGE ( 'NONE', *, *, #19362, .T. ) ;
#17215 = CIRCLE ( 'NONE', #6441, 150.0000000000000284 ) ;
#17217 = DIRECTION ( 'NONE',  ( 0.000000000000000000, -1.000000000000000000, 0.000000000000000000 ) ) ;
#17218 = ORIENTED_EDGE ( 'NONE', *, *, #7233, .T. ) ;
#17219 = CARTESIAN_POINT ( 'NONE',  ( -106.5742148451189877, -120.1859338240075914, 3.408460579751304959E-15 ) ) ;
#17220 = LINE ( 'NONE', #1561, #3806 ) ;
#17221 = ORIENTED_EDGE ( 'NONE', *, *, #6366, .F. ) ;
#17222 = DIRECTION ( 'NONE',  ( 1.000000000000000000, 0.000000000000000000, 0.000000000000000000 ) ) ;
#17223 = CARTESIAN_POINT ( 'NONE',  ( 37.78325588002174840, -47.56406379474564972, 293.5832628385307999 ) ) ;
#17224 = CARTESIAN_POINT ( 'NONE',  ( -97.49999999999997158, -133.9542832455804273, 9.244933322737061587 ) ) ;
#17225 = AXIS2_PLACEMENT_3D ( 'NONE', #487, #7951, #9692 ) ;
#17226 = AXIS2_PLACEMENT_3D ( 'NONE', #11665, #5538, #14644 ) ;
#17227 = CARTESIAN_POINT ( 'NONE',  ( -98.61806909068833704, -132.4668554876671180, 34.59818424444248564 ) ) ;
#17228 = CARTESIAN_POINT ( 'NONE',  ( -7.500000000000001776, 60.00000000000000000, -105.0000000000000142 ) ) ;
#17229 = CARTESIAN_POINT ( 'NONE',  ( -126.6026197240541791, 59.88689088082667666, 35.86430457606912370 ) ) ;
#17230 = AXIS2_PLACEMENT_3D ( 'NONE', #19050, #3487, #3390 ) ;
#17231 = CARTESIAN_POINT ( 'NONE',  ( 97.50000000000002842, -199.9999999999999716, 10.00000000000000178 ) ) ;
#17232 = DIRECTION ( 'NONE',  ( 0.1736481776669306920, -0.9848077530122080203, 0.000000000000000000 ) ) ;
#17233 = DIRECTION ( 'NONE',  ( 1.000000000000000000, 0.000000000000000000, 0.000000000000000000 ) ) ;
#17234 = CARTESIAN_POINT ( 'NONE',  ( -134.3401481871931651, -66.72943863802690601, 37.23267499212099807 ) ) ;
#17235 = EDGE_CURVE ( 'NONE', #11160, #10982, #3833, .T. ) ;
#17236 = EDGE_LOOP ( 'NONE', ( #18414, #5575, #17429, #15884 ) ) ;
#17237 = DIRECTION ( 'NONE',  ( 1.000000000000000000, 0.000000000000000000, 0.000000000000000000 ) ) ;
#17238 = ORIENTED_EDGE ( 'NONE', *, *, #9300, .T. ) ;
#17239 = VERTEX_POINT ( 'NONE', #3063 ) ;
#17240 = AXIS2_PLACEMENT_3D ( 'NONE', #9502, #1720, #3462 ) ;
#17241 = EDGE_CURVE ( 'NONE', #2612, #17735, #15643, .T. ) ;
#17242 = ORIENTED_EDGE ( 'NONE', *, *, #2727, .T. ) ;
#17243 = EDGE_CURVE ( 'NONE', #17330, #8799, #17896, .T. ) ;
#17244 = EDGE_CURVE ( 'NONE', #2173, #14190, #88, .T. ) ;
#17245 = FACE_OUTER_BOUND ( 'NONE', #5860, .T. ) ;
#17246 = CARTESIAN_POINT ( 'NONE',  ( -189.9999999999988916, 275.0000000000000000, -2.499999999999734879 ) ) ;
#17247 = CARTESIAN_POINT ( 'NONE',  ( -15.91767397667354800, 164.0736214083062805, 39.99999999999999289 ) ) ;
#17248 = ORIENTED_EDGE ( 'NONE', *, *, #17180, .T. ) ;
#17249 = CARTESIAN_POINT ( 'NONE',  ( 0.000000000000000000, 0.000000000000000000, 283.5832628385307999 ) ) ;
#17250 = CARTESIAN_POINT ( 'NONE',  ( -134.7188131032333445, -72.93593548660989256, 10.00000000000000178 ) ) ;
#17251 = DIRECTION ( 'NONE',  ( 1.000000000000000000, 0.000000000000000000, -0.000000000000000000 ) ) ;
#17252 = DIRECTION ( 'NONE',  ( 1.000000000000000000, 0.000000000000000000, 0.000000000000000000 ) ) ;
#17253 = CARTESIAN_POINT ( 'NONE',  ( -75.71267875615025389, -86.11264925328200093, 14.88498244535597870 ) ) ;
#17254 = VECTOR ( 'NONE', #11012, 1000.000000000000000 ) ;
#17255 = ADVANCED_FACE ( 'NONE', ( #19025 ), #15741, .T. ) ;
#17256 = VERTEX_POINT ( 'NONE', #18822 ) ;
#17257 = CIRCLE ( 'NONE', #10363, 7.500000000000007105 ) ;
#17258 = CARTESIAN_POINT ( 'NONE',  ( 134.6725548700753734, -73.30144156569930658, 31.86612652126208900 ) ) ;
#17259 = CARTESIAN_POINT ( 'NONE',  ( 133.1916981995338460, -82.53555109165358772, 38.51379023202792951 ) ) ;
#17260 = ORIENTED_EDGE ( 'NONE', *, *, #18462, .T. ) ;
#17261 = ORIENTED_EDGE ( 'NONE', *, *, #16132, .T. ) ;
#17262 = ORIENTED_EDGE ( 'NONE', *, *, #17519, .F. ) ;
#17263 = EDGE_LOOP ( 'NONE', ( #10415, #2314, #9048 ) ) ;
#17264 = LINE ( 'NONE', #14188, #19691 ) ;
#17265 = ADVANCED_FACE ( 'NONE', ( #4805 ), #19121, .T. ) ;
#17266 = ORIENTED_EDGE ( 'NONE', *, *, #9967, .F. ) ;
#17267 = CARTESIAN_POINT ( 'NONE',  ( 67.50000000000000000, 6.284666409917639535E-13, -105.0000000000000142 ) ) ;
#17268 = EDGE_CURVE ( 'NONE', #12685, #5478, #6791, .T. ) ;
#17269 = AXIS2_PLACEMENT_3D ( 'NONE', #18683, #12828, #11089 ) ;
#17270 = ADVANCED_FACE ( 'NONE', ( #14310 ), #187, .T. ) ;
#17271 = DIRECTION ( 'NONE',  ( 0.8479630283625716469, -0.5300553768524345344, 0.000000000000000000 ) ) ;
#17272 = FACE_BOUND ( 'NONE', #13043, .T. ) ;
#17273 = AXIS2_PLACEMENT_3D ( 'NONE', #6770, #3493, #3595 ) ;
#17274 = DIRECTION ( 'NONE',  ( 0.000000000000000000, 0.000000000000000000, -1.000000000000000000 ) ) ;
#17275 = CARTESIAN_POINT ( 'NONE',  ( 77.50000000000000000, 0.000000000000000000, -100.0000000000000000 ) ) ;
#17276 = VERTEX_POINT ( 'NONE', #18925 ) ;
#17277 = DIRECTION ( 'NONE',  ( 0.000000000000000000, 0.000000000000000000, 1.000000000000000000 ) ) ;
#17278 = PLANE ( 'NONE',  #1280 ) ;
#17279 = VERTEX_POINT ( 'NONE', #11127 ) ;
#17280 = DIRECTION ( 'NONE',  ( 0.3747554100459959958, 0.9271237148521535021, 0.000000000000000000 ) ) ;
#17281 = FACE_OUTER_BOUND ( 'NONE', #11753, .T. ) ;
#17282 = CARTESIAN_POINT ( 'NONE',  ( 57.92709869106709419, 18.28567271940532990, 283.5832628385307999 ) ) ;
#17283 = EDGE_CURVE ( 'NONE', #10487, #2923, #14618, .T. ) ;
#17284 = VECTOR ( 'NONE', #12188, 1000.000000000000000 ) ;
#17285 = CARTESIAN_POINT ( 'NONE',  ( 86.01343624116272224, 31.38211805825951473, 30.00000000000000000 ) ) ;
#17286 = DIRECTION ( 'NONE',  ( 0.000000000000000000, 0.000000000000000000, 1.000000000000000000 ) ) ;
#17287 = CARTESIAN_POINT ( 'NONE',  ( 92.21618480002784679, -118.3073397699785829, 47.80227178660424414 ) ) ;
#17288 = AXIS2_PLACEMENT_3D ( 'NONE', #397, #11034, #6553 ) ;
#17289 = CIRCLE ( 'NONE', #7794, 150.0000000000000284 ) ;
#17290 = ORIENTED_EDGE ( 'NONE', *, *, #14739, .F. ) ;
#17291 = VECTOR ( 'NONE', #2228, 1000.000000000000000 ) ;
#17292 = LINE ( 'NONE', #3367, #1755 ) ;
#17293 = EDGE_LOOP ( 'NONE', ( #9716, #5855, #17391, #4418 ) ) ;
#17294 = EDGE_LOOP ( 'NONE', ( #7288, #4666, #5408, #18007 ) ) ;
#17295 = DIRECTION ( 'NONE',  ( 6.982962677686266711E-15, -0.000000000000000000, 1.000000000000000000 ) ) ;
#17296 = ADVANCED_FACE ( 'NONE', ( #9697 ), #15946, .T. ) ;
#17297 = ORIENTED_EDGE ( 'NONE', *, *, #10465, .T. ) ;
#17298 = EDGE_CURVE ( 'NONE', #17394, #16556, #12657, .T. ) ;
#17299 = DIRECTION ( 'NONE',  ( 0.000000000000000000, 1.000000000000000000, 0.000000000000000000 ) ) ;
#17300 = CARTESIAN_POINT ( 'NONE',  ( 113.5802308907675666, 8.308367629983374414, 14.88498244535465709 ) ) ;
#17301 = EDGE_LOOP ( 'NONE', ( #16825, #19228, #10790, #17793 ) ) ;
#17302 = AXIS2_PLACEMENT_3D ( 'NONE', #2984, #13813, #5849 ) ;
#17303 = CARTESIAN_POINT ( 'NONE',  ( 0.8038475772933646457, -10.39230484541326582, 2.804506490479260738E-17 ) ) ;
#17304 = CYLINDRICAL_SURFACE ( 'NONE', #3435, 15.91767397667354089 ) ;
#17305 = CIRCLE ( 'NONE', #19891, 150.0000000000000284 ) ;
#17306 = VECTOR ( 'NONE', #6233, 1000.000000000000000 ) ;
#17307 = EDGE_CURVE ( 'NONE', #18133, #19595, #9798, .T. ) ;
#17308 = EDGE_CURVE ( 'NONE', #625, #10243, #11437, .T. ) ;
#17309 = DIRECTION ( 'NONE',  ( -0.000000000000000000, -0.000000000000000000, -1.000000000000000000 ) ) ;
#17310 = DIRECTION ( 'NONE',  ( 0.000000000000000000, -1.000000000000000000, 0.000000000000000000 ) ) ;
#17311 = ORIENTED_EDGE ( 'NONE', *, *, #19387, .T. ) ;
#17312 = CARTESIAN_POINT ( 'NONE',  ( -15.91767397667354800, 164.0736214083062805, 39.99999999999999289 ) ) ;
#17313 = APPLICATION_CONTEXT ( 'automotive_design' ) ;
#17314 = PLANE ( 'NONE',  #4477 ) ;
#17315 = DIRECTION ( 'NONE',  ( 1.000000000000000000, 0.000000000000000000, -6.976128451377902853E-15 ) ) ;
#17316 = CARTESIAN_POINT ( 'NONE',  ( 84.44144489238081519, -123.9750712224027467, 39.83491645190957797 ) ) ;
#17317 = ORIENTED_EDGE ( 'NONE', *, *, #14655, .T. ) ;
#17318 = CYLINDRICAL_SURFACE ( 'NONE', #6499, 62.91752772691707207 ) ;
#17319 = CARTESIAN_POINT ( 'NONE',  ( -72.27300218572868573, 131.4418965710077885, 18.41322297944785191 ) ) ;
#17320 = VERTEX_POINT ( 'NONE', #17591 ) ;
#17321 = VECTOR ( 'NONE', #18018, 1000.000000000000000 ) ;
#17322 = AXIS2_PLACEMENT_3D ( 'NONE', #2925, #19995, #10680 ) ;
#17323 = ORIENTED_EDGE ( 'NONE', *, *, #2402, .F. ) ;
#17324 = ORIENTED_EDGE ( 'NONE', *, *, #19059, .T. ) ;
#17325 = DIRECTION ( 'NONE',  ( -6.982962677686266711E-15, 0.000000000000000000, -1.000000000000000000 ) ) ;
#17326 = ORIENTED_EDGE ( 'NONE', *, *, #13848, .T. ) ;
#17327 = CARTESIAN_POINT ( 'NONE',  ( -25.74015858913147170, 7.810105800529631992, 39.88498244535563231 ) ) ;
#17328 = B_SPLINE_CURVE_WITH_KNOTS ( 'NONE', 3,
 ( #10328, #13195, #2471, #3708, #10237, #9947, #16198, #16492, #8703, #2083 ),
 .UNSPECIFIED., .F., .F.,
 ( 4, 2, 2, 2, 4 ),
 ( -0.03180955504969720099, -0.02385716628727290248, -0.01590477752484860396, -0.007952388762424298513, 6.938893903907228378E-18 ),
 .UNSPECIFIED. ) ;
#17329 = DIRECTION ( 'NONE',  ( -6.982962677686266711E-15, 0.000000000000000000, -1.000000000000000000 ) ) ;
#17330 = VERTEX_POINT ( 'NONE', #2035 ) ;
#17331 = LINE ( 'NONE', #14041, #3044 ) ;
#17332 = FACE_OUTER_BOUND ( 'NONE', #1118, .T. ) ;
#17333 = CARTESIAN_POINT ( 'NONE',  ( 123.6381990918736449, -84.94542618836281633, 49.99999999999999289 ) ) ;
#17334 = EDGE_CURVE ( 'NONE', #10728, #4820, #19834, .T. ) ;
#17335 = CARTESIAN_POINT ( 'NONE',  ( -104.7061264978949708, -123.3530444481632742, 39.62017787115935619 ) ) ;
#17336 = CARTESIAN_POINT ( 'NONE',  ( 73.25972925305627825, -27.53920554013664912, 132.4711112102474146 ) ) ;
#17337 = CARTESIAN_POINT ( 'NONE',  ( -137.3272859360866676, 27.29364767066081754, 26.87729632077950725 ) ) ;
#17338 = DIRECTION ( 'NONE',  ( -0.8660254037844363761, -0.5000000000000039968, 0.000000000000000000 ) ) ;
#17339 = CARTESIAN_POINT ( 'NONE',  ( -149.9468681919209700, 4.311564970281852816, 2.773916037623369135 ) ) ;
#17340 = CARTESIAN_POINT ( 'NONE',  ( -50.37374754117255549, -141.2886604036510221, 39.99999999999999289 ) ) ;
#17341 = LINE ( 'NONE', #8109, #1017 ) ;
#17342 = CARTESIAN_POINT ( 'NONE',  ( -130.6561114389107274, -73.68416578909176451, 45.68373799725728901 ) ) ;
#17343 = EDGE_LOOP ( 'NONE', ( #6016, #10620, #13514, #9479, #4497 ) ) ;
#17344 = DIRECTION ( 'NONE',  ( 0.000000000000000000, 0.000000000000000000, 1.000000000000000000 ) ) ;
#17345 = AXIS2_PLACEMENT_3D ( 'NONE', #10508, #16764, #4383 ) ;
#17346 = CARTESIAN_POINT ( 'NONE',  ( -82.03124999999998579, -125.5821405433014064, 30.00000000000000000 ) ) ;
#17347 = EDGE_LOOP ( 'NONE', ( #15560, #14369, #10943, #15159 ) ) ;
#17348 = CIRCLE ( 'NONE', #11754, 9.999999999999994671 ) ;
#17349 = ORIENTED_EDGE ( 'NONE', *, *, #11334, .F. ) ;
#17350 = ORIENTED_EDGE ( 'NONE', *, *, #9242, .F. ) ;
#17351 = EDGE_CURVE ( 'NONE', #3741, #10316, #8560, .T. ) ;
#17352 = DIRECTION ( 'NONE',  ( 0.5000000000000101030, -0.8660254037844328234, 0.000000000000000000 ) ) ;
#17353 = DIRECTION ( 'NONE',  ( 1.000000000000000000, 0.000000000000000000, 0.000000000000000000 ) ) ;
#17354 = CARTESIAN_POINT ( 'NONE',  ( -26.55444175050983091, 16.92388544840482112, 248.9926560891072143 ) ) ;
#17355 = CARTESIAN_POINT ( 'NONE',  ( -159.9599531637108782, -36.50981547337168109, 60.00000000000000000 ) ) ;
#17356 = CIRCLE ( 'NONE', #8523, 60.74260934110282051 ) ;
#17357 = DIRECTION ( 'NONE',  ( 1.000000000000000000, 0.000000000000000000, 0.000000000000000000 ) ) ;
#17358 = DIRECTION ( 'NONE',  ( -0.6234898018587431423, 0.7818314824680221431, 0.000000000000000000 ) ) ;
#17359 = CARTESIAN_POINT ( 'NONE',  ( 97.67667160654319503, -133.7228621772585200, 31.88576057819609488 ) ) ;
#17360 = AXIS2_PLACEMENT_3D ( 'NONE', #5080, #6516, #19193 ) ;
#17361 = CARTESIAN_POINT ( 'NONE',  ( 0.000000000000000000, 0.000000000000000000, 283.5832628385307999 ) ) ;
#17362 = ORIENTED_EDGE ( 'NONE', *, *, #12374, .F. ) ;
#17363 = EDGE_CURVE ( 'NONE', #13453, #9086, #5473, .T. ) ;
#17364 = LINE ( 'NONE', #3439, #14320 ) ;
#17365 = DIRECTION ( 'NONE',  ( -1.000000000000000000, 0.000000000000000000, 6.982962677686266711E-15 ) ) ;
#17366 = ORIENTED_EDGE ( 'NONE', *, *, #13385, .F. ) ;
#17367 = EDGE_LOOP ( 'NONE', ( #4943, #7067, #12436, #21 ) ) ;
#17368 = ORIENTED_EDGE ( 'NONE', *, *, #1855, .T. ) ;
#17369 = CARTESIAN_POINT ( 'NONE',  ( 0.000000000000000000, 0.000000000000000000, -10.00000000000000178 ) ) ;
#17370 = AXIS2_PLACEMENT_3D ( 'NONE', #3479, #17508, #5128 ) ;
#17371 = ORIENTED_EDGE ( 'NONE', *, *, #3890, .T. ) ;
#17372 = DIRECTION ( 'NONE',  ( 1.000000000000000000, 0.000000000000000000, 0.000000000000000000 ) ) ;
#17373 = CIRCLE ( 'NONE', #5583, 62.91752772691707207 ) ;
#17374 = EDGE_CURVE ( 'NONE', #13130, #11866, #6421, .T. ) ;
#17375 = CARTESIAN_POINT ( 'NONE',  ( -99.75421581617491995, -130.9036673766147771, 36.36146831168105820 ) ) ;
#17376 =( NAMED_UNIT ( * ) PLANE_ANGLE_UNIT ( ) SI_UNIT ( $, .RADIAN. ) );
#17377 = LINE ( 'NONE', #9787, #19213 ) ;
#17378 = ORIENTED_EDGE ( 'NONE', *, *, #4273, .T. ) ;
#17379 = CARTESIAN_POINT ( 'NONE',  ( -71.18887634719365565, -147.8252249328922687, 60.00000000000000000 ) ) ;
#17380 = DIRECTION ( 'NONE',  ( 0.8660254037844380415, 0.5000000000000009992, 0.000000000000000000 ) ) ;
#17381 = VERTEX_POINT ( 'NONE', #787 ) ;
#17382 = SHAPE_REPRESENTATION ( 'MAS-341', ( #5599, #13384, #9850, #14058, #17666, #4628, #8818, #5252, #16675, #19012, #18022 ), #1306 ) ;
#17383 = CARTESIAN_POINT ( 'NONE',  ( -91.75873705015325754, 111.3640350795034237, -30.64689026788566650 ) ) ;
#17384 = CARTESIAN_POINT ( 'NONE',  ( -59.58067424803613221, 20.21777810286735999, 293.5832628385307999 ) ) ;
#17385 = DIRECTION ( 'NONE',  ( 0.000000000000000000, -0.000000000000000000, 1.000000000000000000 ) ) ;
#17386 = CARTESIAN_POINT ( 'NONE',  ( -115.2828271789296650, -14.71737894807794156, 14.88498244535625759 ) ) ;
#17387 = EDGE_CURVE ( 'NONE', #2503, #5679, #7097, .T. ) ;
#17388 = CARTESIAN_POINT ( 'NONE',  ( 0.000000000000000000, 0.000000000000000000, -110.0000000000000000 ) ) ;
#17389 = LINE ( 'NONE', #1721, #10442 ) ;
#17390 = DIRECTION ( 'NONE',  ( -0.000000000000000000, -0.000000000000000000, -1.000000000000000000 ) ) ;
#17391 = ORIENTED_EDGE ( 'NONE', *, *, #18225, .F. ) ;
#17392 = EDGE_CURVE ( 'NONE', #17037, #19269, #8462, .T. ) ;
#17393 = DIRECTION ( 'NONE',  ( 0.000000000000000000, 0.000000000000000000, 1.000000000000000000 ) ) ;
#17394 = VERTEX_POINT ( 'NONE', #19419 ) ;
#17395 = ORIENTED_EDGE ( 'NONE', *, *, #4478, .T. ) ;
#17396 = PLANE ( 'NONE',  #16118 ) ;
#17397 = B_SPLINE_CURVE_WITH_KNOTS ( 'NONE', 3,
 ( #15014, #2150, #16165, #10114, #7242, #602, #5709, #11825, #8476, #16561, #4065, #6847, #894, #16362, #13071, #16266, #2541, #2247, #11641, #3677, #6945, #5315, #17897, #18090, #11546, #13461, #14911, #14715, #7150, #8770 ),
 .UNSPECIFIED., .F., .F.,
 ( 4, 2, 2, 2, 2, 2, 2, 2, 2, 2, 2, 2, 2, 2, 4 ),
 ( 0.000000000000000000, 0.002172065812121075617, 0.003258098718181600198, 0.004344131624242125213, 0.008688263248484262569, 0.009774296154544809268, 0.01086032906060535250, 0.01303239487272644069, 0.01520446068484753062, 0.01737652649696861881, 0.02172065812121076397, 0.02389272393333180880, 0.02606478974545285016, 0.03040892136969493634, 0.03475305299393702252 ),
 .UNSPECIFIED. ) ;
#17398 = EDGE_LOOP ( 'NONE', ( #6818, #16137 ) ) ;
#17399 = CARTESIAN_POINT ( 'NONE',  ( 5.729042578294149202, 0.2993243175132214717, 293.5832628385307999 ) ) ;
#17400 = EDGE_CURVE ( 'NONE', #2029, #13843, #17784, .T. ) ;
#17401 = DIRECTION ( 'NONE',  ( 0.6427876096865300370, 0.7660444431189858960, 0.000000000000000000 ) ) ;
#17402 = ORIENTED_EDGE ( 'NONE', *, *, #7147, .F. ) ;
#17403 = PRESENTATION_STYLE_ASSIGNMENT (( #1738 ) ) ;
#17404 = DIRECTION ( 'NONE',  ( 0.9848077530122080203, 0.1736481776669306920, 0.000000000000000000 ) ) ;
#17405 = DIRECTION ( 'NONE',  ( 0.000000000000000000, -1.000000000000000000, -3.338476886082585705E-16 ) ) ;
#17406 = VECTOR ( 'NONE', #6739, 1000.000000000000000 ) ;
#17407 = VECTOR ( 'NONE', #4976, 1000.000000000000000 ) ;
#17408 = CARTESIAN_POINT ( 'NONE',  ( 4.811834253409037032, 3.123743752084113812, 283.5832628385307999 ) ) ;
#17409 = PLANE ( 'NONE',  #6371 ) ;
#17410 = VERTEX_POINT ( 'NONE', #5496 ) ;
#17411 = PLANE ( 'NONE',  #7918 ) ;
#17412 = DIRECTION ( 'NONE',  ( -0.9396926207859058744, -0.3420201433256757628, 0.000000000000000000 ) ) ;
#17413 = ADVANCED_FACE ( 'NONE', ( #14702 ), #8361, .T. ) ;
#17414 = VECTOR ( 'NONE', #5548, 1000.000000000000000 ) ;
#17415 = CARTESIAN_POINT ( 'NONE',  ( -63.98537287693041264, 94.20918150411493741, 14.88498244535589876 ) ) ;
#17416 = CARTESIAN_POINT ( 'NONE',  ( 105.2683707665266297, -122.4156632037704071, 39.76425450544135032 ) ) ;
#17417 = EDGE_CURVE ( 'NONE', #9731, #9274, #4507, .T. ) ;
#17418 = AXIS2_PLACEMENT_3D ( 'NONE', #2678, #15349, #9212 ) ;
#17419 = ORIENTED_EDGE ( 'NONE', *, *, #2251, .F. ) ;
#17420 = EDGE_CURVE ( 'NONE', #16902, #1745, #1902, .T. ) ;
#17421 = FACE_OUTER_BOUND ( 'NONE', #7793, .T. ) ;
#17422 = CARTESIAN_POINT ( 'NONE',  ( -81.44151772932448807, 125.9672356422290562, 33.01992119261491609 ) ) ;
#17423 = ORIENTED_EDGE ( 'NONE', *, *, #11873, .F. ) ;
#17424 = ORIENTED_EDGE ( 'NONE', *, *, #19867, .F. ) ;
#17425 = ORIENTED_EDGE ( 'NONE', *, *, #1891, .F. ) ;
#17426 = SHAPE_DEFINITION_REPRESENTATION ( #5092, #13949 ) ;
#17427 = AXIS2_PLACEMENT_3D ( 'NONE', #13405, #16695, #3913 ) ;
#17428 = VECTOR ( 'NONE', #7081, 1000.000000000000000 ) ;
#17429 = ORIENTED_EDGE ( 'NONE', *, *, #17504, .T. ) ;
#17430 = DIRECTION ( 'NONE',  ( -0.000000000000000000, -0.000000000000000000, -1.000000000000000000 ) ) ;
#17431 = CARTESIAN_POINT ( 'NONE',  ( -116.5489102618968360, 94.45925147717298387, 44.49316384199085661 ) ) ;
#17432 = EDGE_CURVE ( 'NONE', #9376, #2619, #1230, .T. ) ;
#17433 = VERTEX_POINT ( 'NONE', #16451 ) ;
#17434 = CIRCLE ( 'NONE', #3369, 106.4288957539800862 ) ;
#17435 = SURFACE_STYLE_USAGE ( .BOTH. , #3798 ) ;
#17436 = DIRECTION ( 'NONE',  ( 1.000000000000000000, 0.000000000000000000, 0.000000000000000000 ) ) ;
#17437 = DIRECTION ( 'NONE',  ( 1.000000000000000000, 0.000000000000000000, 0.000000000000000000 ) ) ;
#17438 = CARTESIAN_POINT ( 'NONE',  ( -95.41207185104575217, -115.7515782192335365, -9.200900026191284553 ) ) ;
#17439 = CARTESIAN_POINT ( 'NONE',  ( 41.06890862491472660, 47.66508197439486594, 132.4711112102474146 ) ) ;
#17440 = DIRECTION ( 'NONE',  ( 0.000000000000000000, 0.000000000000000000, 1.000000000000000000 ) ) ;
#17441 = AXIS2_PLACEMENT_3D ( 'NONE', #1527, #8883, #1429 ) ;
#17442 = VECTOR ( 'NONE', #6723, 1000.000000000000000 ) ;
#17443 = ADVANCED_FACE ( 'NONE', ( #8661 ), #14898, .F. ) ;
#17444 = CYLINDRICAL_SURFACE ( 'NONE', #19326, 62.91752772691707207 ) ;
#17445 = CARTESIAN_POINT ( 'NONE',  ( 0.000000000000000000, 0.000000000000000000, 49.99999999999999289 ) ) ;
#17446 = FACE_BOUND ( 'NONE', #13136, .T. ) ;
#17447 = ORIENTED_EDGE ( 'NONE', *, *, #6051, .T. ) ;
#17448 = CARTESIAN_POINT ( 'NONE',  ( 0.000000000000000000, 0.000000000000000000, 248.9926560891072143 ) ) ;
#17449 = EDGE_CURVE ( 'NONE', #10313, #2962, #16945, .T. ) ;
#17450 = VERTEX_POINT ( 'NONE', #15406 ) ;
#17451 = ORIENTED_EDGE ( 'NONE', *, *, #17779, .F. ) ;
#17452 = AXIS2_PLACEMENT_3D ( 'NONE', #8759, #10195, #6938 ) ;
#17453 = ORIENTED_EDGE ( 'NONE', *, *, #11514, .T. ) ;
#17454 = CARTESIAN_POINT ( 'NONE',  ( -144.0189762191472767, -15.32165204522277868, 13.24322322583874367 ) ) ;
#17455 = DIRECTION ( 'NONE',  ( 1.000000000000000000, 0.000000000000000000, 0.000000000000000000 ) ) ;
#17456 = CARTESIAN_POINT ( 'NONE',  ( -48.17797692984161984, -36.99387960884178028, 293.5832628385307999 ) ) ;
#17457 = AXIS2_PLACEMENT_3D ( 'NONE', #14552, #6783, #19267 ) ;
#17458 = DIRECTION ( 'NONE',  ( -1.000000000000000000, -0.000000000000000000, -0.000000000000000000 ) ) ;
#17459 = CARTESIAN_POINT ( 'NONE',  ( -51.24071425735602503, 32.61983739937743820, 283.5832628385307999 ) ) ;
#17460 = LINE ( 'NONE', #8329, #6939 ) ;
#17461 = CARTESIAN_POINT ( 'NONE',  ( 60.74260934110282051, 0.000000000000000000, 293.5832628385307999 ) ) ;
#17462 = AXIS2_PLACEMENT_3D ( 'NONE', #7436, #10398, #13880 ) ;
#17463 = CARTESIAN_POINT ( 'NONE',  ( 97.53517841124886445, -133.9083944458742224, 30.96027505812804748 ) ) ;
#17464 = CARTESIAN_POINT ( 'NONE',  ( -49.59485801383840453, -102.5175491340983882, 39.88498244535580284 ) ) ;
#17465 = ORIENTED_EDGE ( 'NONE', *, *, #2464, .T. ) ;
#17466 = DIRECTION ( 'NONE',  ( 1.000000000000000000, 0.000000000000000000, 0.000000000000000000 ) ) ;
#17467 = LINE ( 'NONE', #3542, #11645 ) ;
#17468 = ORIENTED_EDGE ( 'NONE', *, *, #17150, .F. ) ;
#17469 = EDGE_LOOP ( 'NONE', ( #1582, #19919 ) ) ;
#17470 = EDGE_LOOP ( 'NONE', ( #15747, #4708, #18723, #7432, #9289 ) ) ;
#17471 = AXIS2_PLACEMENT_3D ( 'NONE', #1564, #12496, #15367 ) ;
#17472 = ORIENTED_EDGE ( 'NONE', *, *, #9863, .T. ) ;
#17473 = PLANE ( 'NONE',  #3703 ) ;
#17474 = AXIS2_PLACEMENT_3D ( 'NONE', #5073, #11297, #11190 ) ;
#17475 = ORIENTED_EDGE ( 'NONE', *, *, #844, .T. ) ;
#17476 = CARTESIAN_POINT ( 'NONE',  ( -110.0000000000000000, 88.56916956954178488, -34.99999999999998579 ) ) ;
#17477 = CARTESIAN_POINT ( 'NONE',  ( -56.84754764479025368, -154.7316448359455308, 60.00000000000000000 ) ) ;
#17478 = DIRECTION ( 'NONE',  ( 0.4693298356057531984, -0.8830229359480288309, 0.000000000000000000 ) ) ;
#17479 = LINE ( 'NONE', #18812, #19519 ) ;
#17480 = VERTEX_POINT ( 'NONE', #981 ) ;
#17481 = CARTESIAN_POINT ( 'NONE',  ( 135.1060089022256818, -65.16414933467422088, 10.00000000000000355 ) ) ;
#17482 = CARTESIAN_POINT ( 'NONE',  ( 138.2024300533213932, 89.85329105948596862, 60.00000000000000000 ) ) ;
#17483 = ORIENTED_EDGE ( 'NONE', *, *, #6721, .F. ) ;
#17484 = FACE_OUTER_BOUND ( 'NONE', #13886, .T. ) ;
#17485 = DIRECTION ( 'NONE',  ( 1.000000000000000000, 0.000000000000000000, 0.000000000000000000 ) ) ;
#17486 = AXIS2_PLACEMENT_3D ( 'NONE', #8383, #6761, #12983 ) ;
#17487 = DIRECTION ( 'NONE',  ( 0.000000000000000000, 0.000000000000000000, -1.000000000000000000 ) ) ;
#17488 = CARTESIAN_POINT ( 'NONE',  ( 1.678175111358115590, 5.485913980968027737, 283.5832628385307999 ) ) ;
#17489 = DIRECTION ( 'NONE',  ( 0.000000000000000000, 0.000000000000000000, 1.000000000000000000 ) ) ;
#17490 = CARTESIAN_POINT ( 'NONE',  ( 90.17913298585700943, -119.8669913176027393, 46.50836399418985678 ) ) ;
#17491 = VERTEX_POINT ( 'NONE', #9057 ) ;
#17492 = EDGE_CURVE ( 'NONE', #18358, #19487, #8736, .T. ) ;
#17493 = CARTESIAN_POINT ( 'NONE',  ( 0.000000000000000000, 0.000000000000000000, 293.5832628385307999 ) ) ;
#17494 = ORIENTED_EDGE ( 'NONE', *, *, #4414, .T. ) ;
#17495 = ORIENTED_EDGE ( 'NONE', *, *, #18046, .F. ) ;
#17496 = CARTESIAN_POINT ( 'NONE',  ( -152.4599531637108498, -36.50981547337168109, 49.99999999999999289 ) ) ;
#17497 = AXIS2_PLACEMENT_3D ( 'NONE', #13473, #16371, #11933 ) ;
#17498 = VERTEX_POINT ( 'NONE', #5799 ) ;
#17499 =( BOUNDED_SURFACE ( )  B_SPLINE_SURFACE ( 3, 2, ( 
 ( #2401, #7003, #853 ),
 ( #5466, #11499, #13222 ),
 ( #8434, #16322, #6907 ),
 ( #2306, #4026, #13319 ),
 ( #14964, #14677, #4124 ),
 ( #8728, #10354, #5373 ),
 ( #16615, #19674, #19577 ),
 ( #5567, #16419, #15068 ),
 ( #8632, #1047, #11692 ),
 ( #7296, #13525, #5274 ),
 ( #17958, #663, #13120 ),
 ( #19386, #11598, #17850 ),
 ( #3827, #3927, #8926 ),
 ( #5770, #18241, #17021 ),
 ( #1467, #1153, #20080 ),
 ( #18555, #7394, #4229 ),
 ( #10661, #15271, #10452 ),
 ( #4537, #13732, #1258 ),
 ( #5974, #2805, #10769 ),
 ( #19873, #3008, #15170 ),
 ( #5874, #13628, #12299 ),
 ( #9237, #4323, #16813 ),
 ( #11987, #16712, #10557 ),
 ( #2697, #9028, #6079 ),
 ( #3111, #15482, #12088 ),
 ( #18348, #7697, #12406 ) ),
 .UNSPECIFIED., .F., .F., .F. ) 
 B_SPLINE_SURFACE_WITH_KNOTS ( ( 4, 2, 2, 2, 2, 2, 2, 2, 2, 2, 2, 2, 4 ),
 ( 3, 3 ),
 ( 0.01017271576669881265, 0.01464115812291478039, 0.01910960047913074986, 0.02134382165723873459, 0.02357804283534671586, 0.02804648519156268532, 0.03028070636967067006, 0.03251492754777865479, 0.03698336990399461732, 0.03921759108210259859, 0.04145181226021058679, 0.04368603343831857500, 0.04592025461642655626 ),
 ( 0.000000000000000000, 1.000000000000000000 ),
 .UNSPECIFIED. ) 
 GEOMETRIC_REPRESENTATION_ITEM ( )  RATIONAL_B_SPLINE_SURFACE ( (
 ( 1.000000000000000000, 0.7071067811865480168, 1.000000000000000000),
 ( 1.000000000000000000, 0.7196766872559550166, 1.000000000000000000),
 ( 1.000000000000000000, 0.7321324053393495346, 1.000000000000000000),
 ( 1.000000000000000000, 0.7567694315053145049, 1.000000000000000000),
 ( 1.000000000000000000, 0.7689510682428757349, 1.000000000000000000),
 ( 1.000000000000000000, 0.7869757430504373819, 1.000000000000000000),
 ( 1.000000000000000000, 0.7929631687995973843, 1.000000000000000000),
 ( 1.000000000000000000, 0.8046623649470893147, 1.000000000000000000),
 ( 1.000000000000000000, 0.8103917441617300987, 1.000000000000000000),
 ( 1.000000000000000000, 0.8272137286302455594, 1.000000000000000000),
 ( 1.000000000000000000, 0.8379439973090835325, 1.000000000000000000),
 ( 1.000000000000000000, 0.8532330560554255428, 1.000000000000000000),
 ( 1.000000000000000000, 0.8581942001721919455, 1.000000000000000000),
 ( 1.000000000000000000, 0.8678183107920264261, 1.000000000000000000),
 ( 1.000000000000000000, 0.8724301636766464974, 1.000000000000000000),
 ( 1.000000000000000000, 0.8855238771547766508, 1.000000000000000000),
 ( 1.000000000000000000, 0.8933247989485895157, 1.000000000000000000),
 ( 1.000000000000000000, 0.9033218449775582970, 1.000000000000000000),
 ( 1.000000000000000000, 0.9063188098299790330, 1.000000000000000000),
 ( 1.000000000000000000, 0.9115443529210249807, 1.000000000000000000),
 ( 1.000000000000000000, 0.9137831556782001208, 1.000000000000000000),
 ( 1.000000000000000000, 0.9174439670357630305, 1.000000000000000000),
 ( 1.000000000000000000, 0.9188661345744038034, 1.000000000000000000),
 ( 1.000000000000000000, 0.9207385544372965747, 1.000000000000000000),
 ( 1.000000000000000000, 0.9212071352555800674, 1.000000000000000000),
 ( 1.000000000000000000, 0.9212076576725564125, 1.000000000000000000) ) ) 
 REPRESENTATION_ITEM ( '' )  SURFACE ( )  );
#17500 = PLANE ( 'NONE',  #6496 ) ;
#17501 = EDGE_CURVE ( 'NONE', #14032, #5816, #4054, .T. ) ;
#17502 = DIRECTION ( 'NONE',  ( -0.000000000000000000, -1.000000000000000000, -0.000000000000000000 ) ) ;
#17503 = ORIENTED_EDGE ( 'NONE', *, *, #5068, .F. ) ;
#17504 = EDGE_CURVE ( 'NONE', #3145, #1943, #12018, .T. ) ;
#17505 = DIRECTION ( 'NONE',  ( 0.9396926207859112035, 0.3420201433256609969, -6.456589605409174593E-15 ) ) ;
#17506 = CARTESIAN_POINT ( 'NONE',  ( 130.9868171408399746, -91.88282611735537841, 50.00000000000000000 ) ) ;
#17507 = EDGE_CURVE ( 'NONE', #10402, #4473, #10384, .T. ) ;
#17508 = DIRECTION ( 'NONE',  ( -0.000000000000000000, -1.000000000000000000, -0.000000000000000000 ) ) ;
#17509 = CYLINDRICAL_SURFACE ( 'NONE', #2911, 62.91752772691707207 ) ;
#17510 = AXIS2_PLACEMENT_3D ( 'NONE', #2344, #7151, #16464 ) ;
#17511 = CARTESIAN_POINT ( 'NONE',  ( 159.9599531637113330, -36.50981547336952104, 60.00000000000000000 ) ) ;
#17512 = DIRECTION ( 'NONE',  ( 0.000000000000000000, 0.000000000000000000, 1.000000000000000000 ) ) ;
#17513 = ORIENTED_EDGE ( 'NONE', *, *, #17876, .F. ) ;
#17514 = CARTESIAN_POINT ( 'NONE',  ( 0.000000000000000000, 0.000000000000000000, 283.5832628385307999 ) ) ;
#17515 = CARTESIAN_POINT ( 'NONE',  ( 170.2125097089226529, -199.3942630591406839, 40.00000000000000000 ) ) ;
#17516 = DIRECTION ( 'NONE',  ( -1.000000000000000000, -0.000000000000000000, -0.000000000000000000 ) ) ;
#17517 = CARTESIAN_POINT ( 'NONE',  ( 0.8038475772933632024, 5.196152422706628471, 9.000000000000001776 ) ) ;
#17518 = EDGE_LOOP ( 'NONE', ( #16717, #10786, #3750, #8320 ) ) ;
#17519 = EDGE_CURVE ( 'NONE', #5404, #14388, #15300, .T. ) ;
#17520 = FACE_OUTER_BOUND ( 'NONE', #18572, .T. ) ;
#17521 = LINE ( 'NONE', #11366, #9899 ) ;
#17522 = VERTEX_POINT ( 'NONE', #16838 ) ;
#17523 = CIRCLE ( 'NONE', #14570, 60.74260934110282051 ) ;
#17524 = VERTEX_POINT ( 'NONE', #7425 ) ;
#17525 = ORIENTED_EDGE ( 'NONE', *, *, #11382, .T. ) ;
#17526 = PRODUCT_CONTEXT ( 'NONE', #14162, 'mechanical' ) ;
#17527 = ADVANCED_BREP_SHAPE_REPRESENTATION ( '', ( #8063, #18639 ), #2627 ) ;
#17528 = VECTOR ( 'NONE', #7847, 1000.000000000000000 ) ;
#17529 = ORIENTED_EDGE ( 'NONE', *, *, #8017, .T. ) ;
#17530 = CARTESIAN_POINT ( 'NONE',  ( 57.94128254008182921, 9.381844291199925578, 132.4711112102474146 ) ) ;
#17531 = LINE ( 'NONE', #15987, #7404 ) ;
#17532 = ORIENTED_EDGE ( 'NONE', *, *, #19270, .F. ) ;
#17533 = EDGE_CURVE ( 'NONE', #16598, #12901, #8951, .T. ) ;
#17534 =( NAMED_UNIT ( * ) SI_UNIT ( $, .STERADIAN. ) SOLID_ANGLE_UNIT ( ) );
#17535 = DIRECTION ( 'NONE',  ( -6.982962677686266711E-15, 0.000000000000000000, -1.000000000000000000 ) ) ;
#17536 = CARTESIAN_POINT ( 'NONE',  ( 134.4038851132261243, -66.60439670040142346, 37.04366817629225039 ) ) ;
#17537 = ADVANCED_FACE ( 'NONE', ( #11914 ), #18938, .F. ) ;
#17538 = VECTOR ( 'NONE', #14719, 1000.000000000000000 ) ;
#17539 = CARTESIAN_POINT ( 'NONE',  ( -136.0833144514123774, 32.93923414480397582, 28.34839128100539440 ) ) ;
#17540 = CIRCLE ( 'NONE', #10319, 7.500000000000008882 ) ;
#17541 = CARTESIAN_POINT ( 'NONE',  ( -2.629250726500700353, -60.68567895461850981, 283.5832628385307999 ) ) ;
#17542 = FACE_OUTER_BOUND ( 'NONE', #1664, .T. ) ;
#17543 = CYLINDRICAL_SURFACE ( 'NONE', #18016, 62.91752772691707207 ) ;
#17544 = DIRECTION ( 'NONE',  ( 1.000000000000000000, 0.000000000000000000, -0.000000000000000000 ) ) ;
#17545 = ORIENTED_EDGE ( 'NONE', *, *, #7274, .T. ) ;
#17546 = AXIS2_PLACEMENT_3D ( 'NONE', #13709, #6160, #1130 ) ;
#17547 = EDGE_CURVE ( 'NONE', #16612, #698, #2540, .T. ) ;
#17548 = CARTESIAN_POINT ( 'NONE',  ( -56.12662799072088404, 23.22641211976270625, 283.5832628385307999 ) ) ;
#17549 = ORIENTED_EDGE ( 'NONE', *, *, #13472, .T. ) ;
#17550 = CIRCLE ( 'NONE', #18861, 7.500000000000007105 ) ;
#17551 = ORIENTED_EDGE ( 'NONE', *, *, #19603, .T. ) ;
#17552 = CIRCLE ( 'NONE', #4136, 60.74260934110282051 ) ;
#17553 = EDGE_LOOP ( 'NONE', ( #18771, #449, #16650, #15849 ) ) ;
#17554 = EDGE_CURVE ( 'NONE', #7714, #6701, #17364, .T. ) ;
#17555 = EDGE_CURVE ( 'NONE', #16780, #9274, #20210, .T. ) ;
#17556 = DIRECTION ( 'NONE',  ( -0.000000000000000000, -0.000000000000000000, 1.000000000000000000 ) ) ;
#17557 = DIRECTION ( 'NONE',  ( -1.000000000000000000, 0.000000000000000000, 0.000000000000000000 ) ) ;
#17558 = DIRECTION ( 'NONE',  ( 0.000000000000000000, 0.000000000000000000, 1.000000000000000000 ) ) ;
#17559 = CARTESIAN_POINT ( 'NONE',  ( -136.4994460260996902, -31.11111111111111782, -9.999999999999987566 ) ) ;
#17560 = EDGE_CURVE ( 'NONE', #3720, #8668, #18585, .T. ) ;
#17561 = CARTESIAN_POINT ( 'NONE',  ( 47.56406379474552182, 37.78325588002191893, 293.5832628385307999 ) ) ;
#17562 = DIRECTION ( 'NONE',  ( 0.9271237148521548344, -0.3747554100459928317, 0.000000000000000000 ) ) ;
#17563 = CARTESIAN_POINT ( 'NONE',  ( -135.1060089022256818, -65.16414933467417825, 30.00000000000000000 ) ) ;
#17564 = DIRECTION ( 'NONE',  ( 0.000000000000000000, 0.8660254037844375974, -0.5000000000000019984 ) ) ;
#17565 = FACE_OUTER_BOUND ( 'NONE', #20110, .T. ) ;
#17566 = EDGE_LOOP ( 'NONE', ( #14616, #2415, #942 ) ) ;
#17567 = CARTESIAN_POINT ( 'NONE',  ( 11.00103590902871353, 57.65577537092163851, 112.0427633081292953 ) ) ;
#17568 = CARTESIAN_POINT ( 'NONE',  ( 134.5351519296996798, -74.34771143809118144, 33.58511643466852092 ) ) ;
#17569 = ORIENTED_EDGE ( 'NONE', *, *, #17746, .T. ) ;
#17571 = ORIENTED_EDGE ( 'NONE', *, *, #5282, .F. ) ;
#17570 = AXIS2_PLACEMENT_3D ( 'NONE', #18503, #18611, #10507 ) ;
#17572 = VECTOR ( 'NONE', #7009, 1000.000000000000227 ) ;
#17573 = ORIENTED_EDGE ( 'NONE', *, *, #168, .F. ) ;
#17574 = EDGE_LOOP ( 'NONE', ( #19226, #1053, #18965, #6445 ) ) ;
#17575 = CARTESIAN_POINT ( 'NONE',  ( -176.7850001792984926, -190.0000000000000284, 33.42750952962406075 ) ) ;
#17576 = VERTEX_POINT ( 'NONE', #18693 ) ;
#17577 = DIRECTION ( 'NONE',  ( 0.000000000000000000, 0.000000000000000000, -1.000000000000000000 ) ) ;
#17578 = CARTESIAN_POINT ( 'NONE',  ( -1.396592535537253342E-14, 0.000000000000000000, 39.88498244535545467 ) ) ;
#17579 = LINE ( 'NONE', #3254, #10248 ) ;
#17580 = LINE ( 'NONE', #14299, #11032 ) ;
#17581 = VERTEX_POINT ( 'NONE', #3038 ) ;
#17582 = CARTESIAN_POINT ( 'NONE',  ( 132.4400928985788539, -70.43137869103952653, -2.824645996396161873 ) ) ;
#17583 = CARTESIAN_POINT ( 'NONE',  ( -22.30005961346265408, -56.50329132715937419, 283.5832628385307999 ) ) ;
#17584 = CIRCLE ( 'NONE', #7110, 60.74260934110282051 ) ;
#17585 = EDGE_LOOP ( 'NONE', ( #18200, #8671, #11556, #6096 ) ) ;
#17586 = CIRCLE ( 'NONE', #18218, 7.500000000000020428 ) ;
#17587 = FACE_OUTER_BOUND ( 'NONE', #7014, .T. ) ;
#17588 = DIRECTION ( 'NONE',  ( -0.000000000000000000, -0.000000000000000000, 1.000000000000000000 ) ) ;
#17589 = DIRECTION ( 'NONE',  ( 0.000000000000000000, 0.000000000000000000, 1.000000000000000000 ) ) ;
#17590 = CARTESIAN_POINT ( 'NONE',  ( 0.8220851292435327196, 78.26059000578311498, 132.4711112102474146 ) ) ;
#17591 = CARTESIAN_POINT ( 'NONE',  ( -176.1792632384392050, -186.5724904703759535, 10.00000000000000178 ) ) ;
#17592 = CARTESIAN_POINT ( 'NONE',  ( -75.09489825810958052, 118.1556484538405414, 7.611160636458589757 ) ) ;
#17593 = ORIENTED_EDGE ( 'NONE', *, *, #12193, .T. ) ;
#17594 = CARTESIAN_POINT ( 'NONE',  ( 51.36153797460909232, -59.06449708980179025, 110.7293897666001214 ) ) ;
#17595 = ORIENTED_EDGE ( 'NONE', *, *, #11395, .F. ) ;
#17596 = ORIENTED_EDGE ( 'NONE', *, *, #6285, .F. ) ;
#17597 = DIRECTION ( 'NONE',  ( 0.000000000000000000, 0.000000000000000000, 1.000000000000000000 ) ) ;
#17598 = AXIS2_PLACEMENT_3D ( 'NONE', #16793, #18536, #2787 ) ;
#17599 = VERTEX_POINT ( 'NONE', #15717 ) ;
#17600 = FACE_OUTER_BOUND ( 'NONE', #2996, .T. ) ;
#17601 = FACE_BOUND ( 'NONE', #11346, .T. ) ;
#17602 = EDGE_LOOP ( 'NONE', ( #5908, #4122, #8399, #2986 ) ) ;
#17603 = CARTESIAN_POINT ( 'NONE',  ( 59.51724408343574879, -12.14957802882732452, 293.5832628385307999 ) ) ;
#17604 = ADVANCED_FACE ( 'NONE', ( #8034 ), #9372, .F. ) ;
#17605 = CARTESIAN_POINT ( 'NONE',  ( 40.27908801169993325, 45.46712722958823605, 283.5832628385307999 ) ) ;
#17606 = CARTESIAN_POINT ( 'NONE',  ( 78.26059000578312919, -0.8220851292427129309, 132.4711112102474146 ) ) ;
#17607 = AXIS2_PLACEMENT_3D ( 'NONE', #16559, #5810, #13673 ) ;
#17608 = CIRCLE ( 'NONE', #8762, 62.91752772691707207 ) ;
#17609 = AXIS2_PLACEMENT_3D ( 'NONE', #13467, #8874, #7155 ) ;
#17610 = LINE ( 'NONE', #16173, #1993 ) ;
#17611 = DIRECTION ( 'NONE',  ( -0.000000000000000000, -0.000000000000000000, 1.000000000000000000 ) ) ;
#17612 = VECTOR ( 'NONE', #4667, 1000.000000000000000 ) ;
#17613 = ORIENTED_EDGE ( 'NONE', *, *, #6227, .T. ) ;
#17614 = DIRECTION ( 'NONE',  ( 0.9396926207859057634, -0.3420201433256757073, -6.561838499445174030E-15 ) ) ;
#17615 = DIRECTION ( 'NONE',  ( 1.000000000000000000, 0.000000000000000000, 0.000000000000000000 ) ) ;
#17616 = DIRECTION ( 'NONE',  ( -0.4693298356057531429, 0.8830229359480288309, 0.000000000000000000 ) ) ;
#17617 = CARTESIAN_POINT ( 'NONE',  ( 96.82170812967342499, -114.6249810635733297, 36.57915001187932091 ) ) ;
#17618 = ORIENTED_EDGE ( 'NONE', *, *, #11813, .T. ) ;
#17619 = EDGE_CURVE ( 'NONE', #3260, #15303, #14635, .T. ) ;
#17620 = DIRECTION ( 'NONE',  ( -0.000000000000000000, -0.000000000000000000, 1.000000000000000000 ) ) ;
#17621 = CARTESIAN_POINT ( 'NONE',  ( -83.84343328673659812, 124.3879646359026623, 35.30785401045157101 ) ) ;
#17622 = ORIENTED_EDGE ( 'NONE', *, *, #10492, .F. ) ;
#17623 = ORIENTED_EDGE ( 'NONE', *, *, #520, .T. ) ;
#17624 = EDGE_CURVE ( 'NONE', #14438, #17628, #19656, .T. ) ;
#17625 = EDGE_LOOP ( 'NONE', ( #8444, #19447, #8427, #10618 ) ) ;
#17626 = SHAPE_DEFINITION_REPRESENTATION ( #4755, #5472 ) ;
#17627 = VECTOR ( 'NONE', #878, 1000.000000000000000 ) ;
#17628 = VERTEX_POINT ( 'NONE', #17940 ) ;
#17629 = CONICAL_SURFACE ( 'NONE', #15984, 9.000000000000000000, 1.047197551196600296 ) ;
#17630 = DIRECTION ( 'NONE',  ( -0.1736481776669273336, 0.9848077530122086864, 1.214091813839188063E-15 ) ) ;
#17631 = AXIS2_PLACEMENT_3D ( 'NONE', #13221, #19481, #8631 ) ;
#17632 = PLANE ( 'NONE',  #12955 ) ;
#17633 = ORIENTED_EDGE ( 'NONE', *, *, #17919, .F. ) ;
#17634 = CARTESIAN_POINT ( 'NONE',  ( -36.66871011346412246, -45.84586732611848703, 132.4711112102474146 ) ) ;
#17635 = DIRECTION ( 'NONE',  ( -0.7660444431189749048, -0.6427876096865430267, 0.000000000000000000 ) ) ;
#17636 = CARTESIAN_POINT ( 'NONE',  ( -98.78543727592952450, -132.2400759706156066, 5.082541774034873505 ) ) ;
#17637 = ADVANCED_FACE ( 'NONE', ( #6988 ), #10058, .T. ) ;
#17638 = CARTESIAN_POINT ( 'NONE',  ( -103.8888757476051836, -46.65403860089418941, 39.88498244535617943 ) ) ;
#17639 = CARTESIAN_POINT ( 'NONE',  ( 128.2779226595531270, 102.2982297021113141, 49.99999999999999289 ) ) ;
#17640 = DIRECTION ( 'NONE',  ( -1.000000000000000000, 0.000000000000000000, 0.000000000000000000 ) ) ;
#17641 = DIRECTION ( 'NONE',  ( 0.9396926207859127578, -0.3420201433256568335, 0.000000000000000000 ) ) ;
#17642 = AXIS2_PLACEMENT_3D ( 'NONE', #5277, #11410, #5079 ) ;
#17643 = FACE_OUTER_BOUND ( 'NONE', #1168, .T. ) ;
#17644 = AXIS2_PLACEMENT_3D ( 'NONE', #13753, #6207, #54 ) ;
#17645 = ORIENTED_EDGE ( 'NONE', *, *, #17084, .F. ) ;
#17646 = ADVANCED_FACE ( 'NONE', ( #1031 ), #11310, .F. ) ;
#17647 = CARTESIAN_POINT ( 'NONE',  ( -113.8386494799486712, 67.89548654814036865, -29.84279094000235233 ) ) ;
#17648 = ADVANCED_FACE ( 'NONE', ( #19559 ), #2293, .T. ) ;
#17649 = EDGE_CURVE ( 'NONE', #383, #1323, #2481, .T. ) ;
#17650 = ORIENTED_EDGE ( 'NONE', *, *, #19375, .F. ) ;
#17651 = ORIENTED_EDGE ( 'NONE', *, *, #262, .F. ) ;
#17652 = VERTEX_POINT ( 'NONE', #8521 ) ;
#17653 = LINE ( 'NONE', #10160, #3717 ) ;
#17654 = VECTOR ( 'NONE', #754, 1000.000000000000000 ) ;
#17655 = EDGE_CURVE ( 'NONE', #17163, #17877, #13504, .T. ) ;
#17656 = CARTESIAN_POINT ( 'NONE',  ( 0.000000000000000000, 0.000000000000000000, 283.5832628385307999 ) ) ;
#17657 = DIRECTION ( 'NONE',  ( -6.982962677686266711E-15, 0.000000000000000000, -1.000000000000000000 ) ) ;
#17658 = DIRECTION ( 'NONE',  ( 0.5000000000000039968, 0.8660254037844362651, -4.304393070272777803E-15 ) ) ;
#17659 = DIRECTION ( 'NONE',  ( -0.000000000000000000, -0.000000000000000000, 1.000000000000000000 ) ) ;
#17660 = CYLINDRICAL_SURFACE ( 'NONE', #13669, 15.91767397667354089 ) ;
#17661 = CARTESIAN_POINT ( 'NONE',  ( 73.25972925305627825, -27.53920554013664912, 111.4180192758974499 ) ) ;
#17662 = CARTESIAN_POINT ( 'NONE',  ( 1.678175111358173099, 5.485913980968232018, 293.5832628385307999 ) ) ;
#17663 = PLANE ( 'NONE',  #682 ) ;
#17664 = DIRECTION ( 'NONE',  ( -0.000000000000000000, -0.000000000000000000, 1.000000000000000000 ) ) ;
#17665 = ORIENTED_EDGE ( 'NONE', *, *, #14125, .F. ) ;
#17666 = AXIS2_PLACEMENT_3D ( 'NONE', #6476, #15682, #10754 ) ;
#17667 = ADVANCED_FACE ( 'NONE', ( #4207 ), #14756, .T. ) ;
#17668 = CIRCLE ( 'NONE', #1655, 7.500000000000020428 ) ;
#17669 = DIRECTION ( 'NONE',  ( 1.000000000000000000, 0.000000000000000000, -0.000000000000000000 ) ) ;
#17670 = ORIENTED_EDGE ( 'NONE', *, *, #12070, .F. ) ;
#17671 = EDGE_CURVE ( 'NONE', #13051, #16478, #17586, .T. ) ;
#17672 = ORIENTED_EDGE ( 'NONE', *, *, #16512, .T. ) ;
#17673 = ORIENTED_EDGE ( 'NONE', *, *, #12912, .T. ) ;
#17674 = ORIENTED_EDGE ( 'NONE', *, *, #1523, .F. ) ;
#17675 = DIRECTION ( 'NONE',  ( -1.000000000000000000, 0.000000000000000000, 0.000000000000000000 ) ) ;
#17676 = PRODUCT_DEFINITION_SHAPE ( 'NONE', 'NONE',  #20245 ) ;
#17677 = ORIENTED_EDGE ( 'NONE', *, *, #7361, .T. ) ;
#17678 = DIRECTION ( 'NONE',  ( 0.000000000000000000, 1.000000000000000000, 0.000000000000000000 ) ) ;
#17679 = CARTESIAN_POINT ( 'NONE',  ( 1.396592535537252080E-14, 0.000000000000000000, 49.99999999999998579 ) ) ;
#17680 = DIRECTION ( 'NONE',  ( 1.000000000000000000, 0.000000000000000000, 0.000000000000000000 ) ) ;
#17681 = DIRECTION ( 'NONE',  ( -1.000000000000000000, 0.000000000000000000, 6.969309079188926949E-15 ) ) ;
#17682 = EDGE_LOOP ( 'NONE', ( #19020, #18507, #6219, #14083 ) ) ;
#17683 = CIRCLE ( 'NONE', #18984, 150.0000000000000284 ) ;
#17684 = CARTESIAN_POINT ( 'NONE',  ( 59.39925916207545242, 20.74471755083624203, 293.5832628385307999 ) ) ;
#17685 = CARTESIAN_POINT ( 'NONE',  ( 5.281164089014835028, 2.240720816136097859, 293.5832628385307999 ) ) ;
#17686 = ORIENTED_EDGE ( 'NONE', *, *, #16188, .F. ) ;
#17687 = CARTESIAN_POINT ( 'NONE',  ( -103.3159608135122767, 96.92777072167388042, -34.47331703024818239 ) ) ;
#17688 = DIRECTION ( 'NONE',  ( 0.000000000000000000, -0.000000000000000000, 1.000000000000000000 ) ) ;
#17689 = DIRECTION ( 'NONE',  ( -0.6427876096865405842, 0.7660444431189771253, 0.000000000000000000 ) ) ;
#17690 = DIRECTION ( 'NONE',  ( 0.6427876096865481337, -0.7660444431189707970, 0.000000000000000000 ) ) ;
#17691 = EDGE_CURVE ( 'NONE', #16123, #15218, #17914, .T. ) ;
#17692 = DIRECTION ( 'NONE',  ( 0.000000000000000000, 0.000000000000000000, -1.000000000000000000 ) ) ;
#17693 = FACE_BOUND ( 'NONE', #15774, .T. ) ;
#17694 = CARTESIAN_POINT ( 'NONE',  ( 82.61717615486089983, -125.1974987762634299, 34.97368933229491716 ) ) ;
#17695 = EDGE_LOOP ( 'NONE', ( #4363, #16140, #18825, #11894 ) ) ;
#17696 = AXIS2_PLACEMENT_3D ( 'NONE', #7523, #9367, #15611 ) ;
#17697 = CARTESIAN_POINT ( 'NONE',  ( -110.0000000000000284, 101.9803902718557111, 44.99999999999998579 ) ) ;
#17698 = ORIENTED_EDGE ( 'NONE', *, *, #16379, .F. ) ;
#17699 = EDGE_CURVE ( 'NONE', #1187, #648, #2681, .T. ) ;
#17700 = VERTEX_POINT ( 'NONE', #5452 ) ;
#17701 = CARTESIAN_POINT ( 'NONE',  ( -12.78021302872797449, 77.21438937758516374, 132.4711112102474146 ) ) ;
#17702 = VERTEX_POINT ( 'NONE', #2382 ) ;
#17703 = PLANE ( 'NONE',  #12351 ) ;
#17704 = CARTESIAN_POINT ( 'NONE',  ( -27.53920554013687649, -73.25972925305620720, 111.4180192758973931 ) ) ;
#17705 = CARTESIAN_POINT ( 'NONE',  ( 0.1469846612282495468, -8.891930899535427812, -2.598723904613008617 ) ) ;
#17706 = CARTESIAN_POINT ( 'NONE',  ( 0.000000000000000000, 0.000000000000000000, 132.4711112102474146 ) ) ;
#17707 = CARTESIAN_POINT ( 'NONE',  ( 7.500000000000420997, -60.00000000000000000, -105.0000000000000142 ) ) ;
#17708 = FACE_OUTER_BOUND ( 'NONE', #14849, .T. ) ;
#17709 = CARTESIAN_POINT ( 'NONE',  ( 62.91215678473958661, -0.8220851292428736912, 248.9926560891072143 ) ) ;
#17710 = DIRECTION ( 'NONE',  ( 0.1736481776669374366, -0.9848077530122066880, 0.000000000000000000 ) ) ;
#17711 = CARTESIAN_POINT ( 'NONE',  ( -49.24833719034228352, -60.83768308848360817, 110.7293897666001214 ) ) ;
#17712 = CARTESIAN_POINT ( 'NONE',  ( -159.9599531637108782, -36.50981547337168109, 60.00000000000000000 ) ) ;
#17713 = DIRECTION ( 'NONE',  ( -0.2225209339563047894, -0.9749279121818258398, 0.000000000000000000 ) ) ;
#17714 = CARTESIAN_POINT ( 'NONE',  ( 95.40880945838065941, -115.7543288757354105, -9.200166993891775391 ) ) ;
#17715 = CARTESIAN_POINT ( 'NONE',  ( 53.87178215532755132, 28.06680738835045119, 293.5832628385307999 ) ) ;
#17716 = EDGE_LOOP ( 'NONE', ( #11586, #711, #11472, #18800 ) ) ;
#17717 = DIRECTION ( 'NONE',  ( -1.000000000000000000, 0.000000000000000000, 0.000000000000000000 ) ) ;
#17718 = CARTESIAN_POINT ( 'NONE',  ( 0.000000000000000000, 0.000000000000000000, 132.4711112102474146 ) ) ;
#17719 = ORIENTED_EDGE ( 'NONE', *, *, #18646, .T. ) ;
#17720 = ORIENTED_EDGE ( 'NONE', *, *, #6857, .T. ) ;
#17721 = ORIENTED_EDGE ( 'NONE', *, *, #19139, .T. ) ;
#17722 = SHAPE_DEFINITION_REPRESENTATION ( #7837, #7558 ) ;
#17723 = ORIENTED_EDGE ( 'NONE', *, *, #2756, .T. ) ;
#17724 = CARTESIAN_POINT ( 'NONE',  ( -125.3183776508946181, 82.47019060060657125, 41.98005522159012770 ) ) ;
#17725 = VERTEX_POINT ( 'NONE', #8616 ) ;
#17726 = AXIS2_PLACEMENT_3D ( 'NONE', #7808, #6389, #1875 ) ;
#17727 = LINE ( 'NONE', #3605, #6658 ) ;
#17728 = DIRECTION ( 'NONE',  ( -6.982962677686266711E-15, 0.000000000000000000, -1.000000000000000000 ) ) ;
#17729 = CARTESIAN_POINT ( 'NONE',  ( -96.25554516485779288, -115.9717118653566388, 9.976009158364529839 ) ) ;
#17730 = ORIENTED_EDGE ( 'NONE', *, *, #18888, .F. ) ;
#17731 = DIRECTION ( 'NONE',  ( 6.982962677686266711E-15, 0.000000000000000000, 1.000000000000000000 ) ) ;
#17732 = CARTESIAN_POINT ( 'NONE',  ( 126.5370453525553671, 80.55045718954892209, 60.00000000000000000 ) ) ;
#17733 = DIRECTION ( 'NONE',  ( 0.000000000000000000, 0.000000000000000000, 1.000000000000000000 ) ) ;
#17734 = DIRECTION ( 'NONE',  ( -0.000000000000000000, 1.000000000000000000, -0.000000000000000000 ) ) ;
#17735 = VERTEX_POINT ( 'NONE', #835 ) ;
#17736 = CARTESIAN_POINT ( 'NONE',  ( 12.23146955673593972, 77.31114765718498916, 248.9926560891072143 ) ) ;
#17737 = VECTOR ( 'NONE', #15594, 1000.000000000000114 ) ;
#17738 = EDGE_CURVE ( 'NONE', #6114, #13453, #7088, .T. ) ;
#17739 = EDGE_CURVE ( 'NONE', #12589, #2533, #18226, .T. ) ;
#17740 = VERTEX_POINT ( 'NONE', #10244 ) ;
#17741 = VECTOR ( 'NONE', #7084, 999.9999999999998863 ) ;
#17742 = ORIENTED_EDGE ( 'NONE', *, *, #4132, .T. ) ;
#17743 = ORIENTED_EDGE ( 'NONE', *, *, #18300, .T. ) ;
#17744 = DIRECTION ( 'NONE',  ( -6.982962677686266711E-15, 0.000000000000000000, -1.000000000000000000 ) ) ;
#17745 = CARTESIAN_POINT ( 'NONE',  ( -129.2265855148631033, -76.16362387560155867, -7.281016149904609769 ) ) ;
#17746 = EDGE_CURVE ( 'NONE', #1319, #11007, #17257, .T. ) ;
#17747 = VECTOR ( 'NONE', #2885, 1000.000000000000000 ) ;
#17748 = CARTESIAN_POINT ( 'NONE',  ( -60.47951622432784546, -49.67518383744813804, 248.9926560891072143 ) ) ;
#17749 = AXIS2_PLACEMENT_3D ( 'NONE', #14140, #10760, #18858 ) ;
#17750 = EDGE_CURVE ( 'NONE', #17450, #3588, #15280, .T. ) ;
#17751 = CARTESIAN_POINT ( 'NONE',  ( -136.3148177136730794, -31.14249925903075678, -13.32260370553848539 ) ) ;
#17752 = EDGE_CURVE ( 'NONE', #15057, #10957, #8426, .T. ) ;
#17753 = CARTESIAN_POINT ( 'NONE',  ( 48.72193424476451185, 39.80940113486035159, 132.4711112102474146 ) ) ;
#17754 = CARTESIAN_POINT ( 'NONE',  ( 55.62246070845780110, -18.77710619359098132, 132.4711112102474146 ) ) ;
#17755 = DIRECTION ( 'NONE',  ( -0.000000000000000000, -0.000000000000000000, 1.000000000000000000 ) ) ;
#17756 = DIRECTION ( 'NONE',  ( -0.000000000000000000, 0.000000000000000000, -1.000000000000000000 ) ) ;
#17757 = VECTOR ( 'NONE', #20116, 1000.000000000000000 ) ;
#17758 = CARTESIAN_POINT ( 'NONE',  ( 98.17232476721000012, -133.0668712321317741, 33.62904428466136153 ) ) ;
#17759 = LINE ( 'NONE', #5082, #3526 ) ;
#17760 = ORIENTED_EDGE ( 'NONE', *, *, #5846, .T. ) ;
#17761 = AXIS2_PLACEMENT_3D ( 'NONE', #12266, #14009, #4605 ) ;
#17762 = ORIENTED_EDGE ( 'NONE', *, *, #2613, .T. ) ;
#17763 = EDGE_CURVE ( 'NONE', #7735, #2759, #18, .T. ) ;
#17764 = VERTEX_POINT ( 'NONE', #7573 ) ;
#17765 = VECTOR ( 'NONE', #16768, 1000.000000000000000 ) ;
#17766 = ORIENTED_EDGE ( 'NONE', *, *, #4993, .T. ) ;
#17767 = ORIENTED_EDGE ( 'NONE', *, *, #3533, .T. ) ;
#17768 = ORIENTED_EDGE ( 'NONE', *, *, #10493, .F. ) ;
#17769 = CIRCLE ( 'NONE', #7958, 79.75827554147308263 ) ;
#17770 = CARTESIAN_POINT ( 'NONE',  ( 71.18887634719571622, -147.8252249328912740, 49.99999999999999289 ) ) ;
#17771 = LINE ( 'NONE', #8549, #16154 ) ;
#17772 = AXIS2_PLACEMENT_3D ( 'NONE', #3375, #11141, #19038 ) ;
#17773 = CARTESIAN_POINT ( 'NONE',  ( -166.7850001792984926, -200.0000000000000284, 40.00000000000000000 ) ) ;
#17774 = VERTEX_POINT ( 'NONE', #13714 ) ;
#17775 = ADVANCED_FACE ( 'NONE', ( #5956 ), #7475, .F. ) ;
#17776 = CARTESIAN_POINT ( 'NONE',  ( 36.99514631729018532, -48.17959877923561862, 293.5832628385307999 ) ) ;
#17777 = DIRECTION ( 'NONE',  ( 0.000000000000000000, 0.000000000000000000, 1.000000000000000000 ) ) ;
#17778 = EDGE_CURVE ( 'NONE', #10931, #12690, #1449, .T. ) ;
#17779 = EDGE_CURVE ( 'NONE', #14411, #9076, #893, .T. ) ;
#17780 = VERTEX_POINT ( 'NONE', #6271 ) ;
#17781 = CARTESIAN_POINT ( 'NONE',  ( -101.6560149856525612, 99.01817082827582794, -34.15757780977866531 ) ) ;
#17782 = CARTESIAN_POINT ( 'NONE',  ( -30.09424155357359254, 27.05260723904714837, 248.9926560891072143 ) ) ;
#17783 = CARTESIAN_POINT ( 'NONE',  ( -21.73104181959829617, -16.26654594725003733, 39.88498244535560389 ) ) ;
#17784 = LINE ( 'NONE', #14507, #3525 ) ;
#17785 = VECTOR ( 'NONE', #16301, 1000.000000000000000 ) ;
#17786 = FACE_OUTER_BOUND ( 'NONE', #9026, .T. ) ;
#17787 = CARTESIAN_POINT ( 'NONE',  ( -63.98537287693041264, 94.20918150411493741, 14.88498244535589876 ) ) ;
#17788 = ORIENTED_EDGE ( 'NONE', *, *, #15036, .T. ) ;
#17789 = ADVANCED_FACE ( 'NONE', ( #17002 ), #12384, .T. ) ;
#17790 = CARTESIAN_POINT ( 'NONE',  ( -152.4599531637108498, -36.50981547337168109, 60.00000000000000000 ) ) ;
#17791 = VECTOR ( 'NONE', #15393, 1000.000000000000000 ) ;
#17792 = VERTEX_POINT ( 'NONE', #18745 ) ;
#17793 = ORIENTED_EDGE ( 'NONE', *, *, #4503, .F. ) ;
#17794 = DIRECTION ( 'NONE',  ( 0.8660254037844363761, 0.5000000000000039968, 0.000000000000000000 ) ) ;
#17795 = ORIENTED_EDGE ( 'NONE', *, *, #12462, .T. ) ;
#17796 = DIRECTION ( 'NONE',  ( -0.000000000000000000, -0.000000000000000000, 1.000000000000000000 ) ) ;
#17797 = CARTESIAN_POINT ( 'NONE',  ( -110.0000000000000142, 1.592040838891559450E-14, -49.99999999999999289 ) ) ;
#17798 = ADVANCED_FACE ( 'NONE', ( #18331 ), #12480, .F. ) ;
#17799 = EDGE_CURVE ( 'NONE', #10010, #20213, #4621, .T. ) ;
#17800 = VECTOR ( 'NONE', #6358, 1000.000000000000000 ) ;
#17801 = DIRECTION ( 'NONE',  ( 6.982962677686266711E-15, -0.000000000000000000, 1.000000000000000000 ) ) ;
#17802 = CARTESIAN_POINT ( 'NONE',  ( 0.000000000000000000, 0.000000000000000000, 293.5832628385307999 ) ) ;
#17803 = EDGE_LOOP ( 'NONE', ( #10091, #7968 ) ) ;
#17804 = DIRECTION ( 'NONE',  ( -0.9781142164131917394, 0.2080686897406911207, 0.000000000000000000 ) ) ;
#17805 = CARTESIAN_POINT ( 'NONE',  ( 20.74471755083603952, -59.39925916207552348, 293.5832628385307999 ) ) ;
#17806 = EDGE_CURVE ( 'NONE', #5943, #166, #13816, .T. ) ;
#17807 = LINE ( 'NONE', #14822, #2641 ) ;
#17808 = DIRECTION ( 'NONE',  ( -0.8830229359480288309, -0.4693298356057531984, 0.000000000000000000 ) ) ;
#17809 = ORIENTED_EDGE ( 'NONE', *, *, #7993, .F. ) ;
#17810 = CARTESIAN_POINT ( 'NONE',  ( 128.2779226595531270, 102.2982297021113141, 39.99999999999999289 ) ) ;
#17811 = CARTESIAN_POINT ( 'NONE',  ( 87.10655032386927132, -147.8252249328912740, 39.99999999999999289 ) ) ;
#17812 = CARTESIAN_POINT ( 'NONE',  ( -38.41834839689332171, 68.18670162478844077, 132.4711112102474146 ) ) ;
#17813 = CIRCLE ( 'NONE', #3747, 140.0000000000000000 ) ;
#17814 = FACE_OUTER_BOUND ( 'NONE', #1141, .T. ) ;
#17815 = VERTEX_POINT ( 'NONE', #2988 ) ;
#17816 = DIRECTION ( 'NONE',  ( 1.000000000000000000, 0.000000000000000000, 0.000000000000000000 ) ) ;
#17817 = CARTESIAN_POINT ( 'NONE',  ( -5.590028426173819120, -1.289614712049182321, 293.5832628385307999 ) ) ;
#17818 = ORIENTED_EDGE ( 'NONE', *, *, #15149, .T. ) ;
#17819 = AXIS2_PLACEMENT_3D ( 'NONE', #14919, #613, #6856 ) ;
#17820 = ORIENTED_EDGE ( 'NONE', *, *, #19165, .F. ) ;
#17821 = ORIENTED_EDGE ( 'NONE', *, *, #2128, .F. ) ;
#17822 = DIRECTION ( 'NONE',  ( -0.9848077530122062440, -0.1736481776669404620, 0.000000000000000000 ) ) ;
#17823 = CARTESIAN_POINT ( 'NONE',  ( 140.0000000000000000, 0.000000000000000000, 49.99999999999999289 ) ) ;
#17824 = ORIENTED_EDGE ( 'NONE', *, *, #7361, .F. ) ;
#17825 = AXIS2_PLACEMENT_3D ( 'NONE', #14621, #16365, #13073 ) ;
#17826 = CARTESIAN_POINT ( 'NONE',  ( 18.92519137117231054, 56.02932139001904233, 248.9926560891072143 ) ) ;
#17827 = CARTESIAN_POINT ( 'NONE',  ( 0.000000000000000000, 7.794228634059941818, 4.500000000000007994 ) ) ;
#17828 = CARTESIAN_POINT ( 'NONE',  ( -96.53160196461145404, -115.8699919790248458, 10.20159961589317632 ) ) ;
#17829 = ORIENTED_EDGE ( 'NONE', *, *, #10467, .T. ) ;
#17830 = CARTESIAN_POINT ( 'NONE',  ( -85.33507189799759374, -123.3618359587738240, -1.358392269459132162 ) ) ;
#17831 = DIRECTION ( 'NONE',  ( -0.5000000000000009992, 0.8660254037844380415, 0.000000000000000000 ) ) ;
#17832 = CARTESIAN_POINT ( 'NONE',  ( -107.4999999999999716, -118.5063289449133634, 50.00000000000000000 ) ) ;
#17833 = LINE ( 'NONE', #736, #16026 ) ;
#17834 = DIRECTION ( 'NONE',  ( -0.000000000000000000, -0.000000000000000000, 1.000000000000000000 ) ) ;
#17835 = CARTESIAN_POINT ( 'NONE',  ( 50.37374754117451658, -141.2886604036503115, 49.99999999999999289 ) ) ;
#17836 = AXIS2_PLACEMENT_3D ( 'NONE', #18178, #16739, #19702 ) ;
#17837 = VERTEX_POINT ( 'NONE', #12067 ) ;
#17838 = DIRECTION ( 'NONE',  ( 0.6427876096865405842, -0.7660444431189771253, -0.000000000000000000 ) ) ;
#17839 = MECHANICAL_DESIGN_GEOMETRIC_PRESENTATION_REPRESENTATION (  '', ( #10625 ), #837 ) ;
#17840 = ORIENTED_EDGE ( 'NONE', *, *, #3016, .F. ) ;
#17841 = VERTEX_POINT ( 'NONE', #1553 ) ;
#17842 = DIRECTION ( 'NONE',  ( 0.2225209339563044841, 0.9749279121818258398, 0.000000000000000000 ) ) ;
#17843 = CIRCLE ( 'NONE', #12938, 150.0000000000000284 ) ;
#17844 = CARTESIAN_POINT ( 'NONE',  ( -133.7387326730402606, -67.93012127445986437, 0.4342299613749713849 ) ) ;
#17845 = DIRECTION ( 'NONE',  ( 0.7430374143461878633, -0.6692498792541777819, 0.000000000000000000 ) ) ;
#17846 = DIRECTION ( 'NONE',  ( -0.7660444431189770143, 0.6427876096865404731, 5.346191897317644012E-15 ) ) ;
#17847 = EDGE_CURVE ( 'NONE', #20212, #9275, #17211, .T. ) ;
#17848 = VECTOR ( 'NONE', #4954, 1000.000000000000000 ) ;
#17849 = CARTESIAN_POINT ( 'NONE',  ( 128.2779226595531270, 102.2982297021113141, 39.99999999999999289 ) ) ;
#17850 = CARTESIAN_POINT ( 'NONE',  ( -133.7753978164293756, -79.32938232250573662, 2.776447817717049737 ) ) ;
#17851 = DIRECTION ( 'NONE',  ( -0.9781142164131917394, 0.2080686897406911207, 0.000000000000000000 ) ) ;
#17852 = DIRECTION ( 'NONE',  ( 1.000000000000000000, 0.000000000000000000, 0.000000000000000000 ) ) ;
#17853 = DIRECTION ( 'NONE',  ( -0.000000000000000000, -0.000000000000000000, 1.000000000000000000 ) ) ;
#17854 = PRODUCT_DEFINITION_CONTEXT ( 'detailed design', #5678, 'design' ) ;
#17855 = ORIENTED_EDGE ( 'NONE', *, *, #9875, .T. ) ;
#17856 = B_SPLINE_CURVE_WITH_KNOTS ( 'NONE', 3,
 ( #13466, #14915, #15019, #4174, #5817, #5419, #16756, #15113, #16368, #19527, #803, #2545, #12035, #10501, #8873, #5516, #7246, #2749, #19718, #3970, #17903, #902, #7154, #13372, #18298, #16566 ),
 .UNSPECIFIED., .F., .F.,
 ( 4, 2, 2, 2, 2, 2, 2, 2, 2, 2, 2, 2, 4 ),
 ( 0.000000000000000000, 0.004334419010351028140, 0.006501628515526520526, 0.008668838020702012911, 0.01300325703105300115, 0.01517046653622849614, 0.01733767604140399113, 0.02167209505175500192, 0.02383930455693049691, 0.02600651406210598496, 0.02817372356728147648, 0.03034093307245696453, 0.03467535208280796144 ),
 .UNSPECIFIED. ) ;
#17857 = EDGE_CURVE ( 'NONE', #9195, #1303, #6801, .T. ) ;
#17858 = VECTOR ( 'NONE', #19437, 1000.000000000000227 ) ;
#17859 = ORIENTED_EDGE ( 'NONE', *, *, #1393, .T. ) ;
#17860 = AXIS2_PLACEMENT_3D ( 'NONE', #19863, #17577, #1039 ) ;
#17861 = ADVANCED_FACE ( 'NONE', ( #15354 ), #6166, .F. ) ;
#17862 = ORIENTED_EDGE ( 'NONE', *, *, #4627, .F. ) ;
#17863 = ADVANCED_FACE ( 'NONE', ( #17100 ), #11698, .T. ) ;
#17864 = EDGE_LOOP ( 'NONE', ( #8938, #7655, #15705 ) ) ;
#17865 = ADVANCED_FACE ( 'NONE', ( #12280 ), #4724, .F. ) ;
#17866 = DIRECTION ( 'NONE',  ( 1.000000000000000000, 0.000000000000000000, 0.000000000000000000 ) ) ;
#17867 = CIRCLE ( 'NONE', #4444, 150.0000000000000284 ) ;
#17868 = ORIENTED_EDGE ( 'NONE', *, *, #19544, .F. ) ;
#17869 = DIRECTION ( 'NONE',  ( -0.6427876096865404731, 0.7660444431189771253, 0.000000000000000000 ) ) ;
#17870 = CARTESIAN_POINT ( 'NONE',  ( 0.4239815141812912636, -0.2650276884262227628, 283.5832628385307999 ) ) ;
#17871 = PLANE ( 'NONE',  #19227 ) ;
#17872 = VERTEX_POINT ( 'NONE', #10950 ) ;
#17873 = CARTESIAN_POINT ( 'NONE',  ( -71.18887634719365565, -147.8252249328922687, 60.00000000000000000 ) ) ;
#17874 = DIRECTION ( 'NONE',  ( 0.000000000000000000, 0.000000000000000000, -1.000000000000000000 ) ) ;
#17875 = VECTOR ( 'NONE', #10683, 1000.000000000000000 ) ;
#17876 = EDGE_CURVE ( 'NONE', #15471, #7939, #4514, .T. ) ;
#17877 = VERTEX_POINT ( 'NONE', #10748 ) ;
#17878 = CARTESIAN_POINT ( 'NONE',  ( -29.99999999999887379, 275.0000000000000000, -2.500000000000847766 ) ) ;
#17879 = CARTESIAN_POINT ( 'NONE',  ( -78.26059000578311498, 0.8220851292432551638, 132.4711112102474146 ) ) ;
#17880 = DIRECTION ( 'NONE',  ( -1.000000000000000000, -0.000000000000000000, -0.000000000000000000 ) ) ;
#17881 = DIRECTION ( 'NONE',  ( -0.000000000000000000, -0.000000000000000000, 1.000000000000000000 ) ) ;
#17882 = VECTOR ( 'NONE', #10310, 1000.000000000000114 ) ;
#17883 = DIRECTION ( 'NONE',  ( 0.000000000000000000, -0.000000000000000000, -1.000000000000000000 ) ) ;
#17884 = CARTESIAN_POINT ( 'NONE',  ( -110.0000000000000142, 275.0000000000000000, -75.00000000000000000 ) ) ;
#17885 = DIRECTION ( 'NONE',  ( 0.1736481776669241417, 0.9848077530122091305, 0.000000000000000000 ) ) ;
#17886 = EDGE_LOOP ( 'NONE', ( #19613, #3573, #571, #10886 ) ) ;
#17887 = ADVANCED_FACE ( 'NONE', ( #15250 ), #1236, .T. ) ;
#17888 = CARTESIAN_POINT ( 'NONE',  ( 7.350000000000000533, 9.000000000000000000, 0.000000000000000000 ) ) ;
#17889 = ORIENTED_EDGE ( 'NONE', *, *, #12490, .T. ) ;
#17890 = EDGE_CURVE ( 'NONE', #13973, #4841, #15673, .T. ) ;
#17891 = ORIENTED_EDGE ( 'NONE', *, *, #731, .T. ) ;
#17892 = EDGE_CURVE ( 'NONE', #15414, #3831, #11047, .T. ) ;
#17893 = DIRECTION ( 'NONE',  ( 0.000000000000000000, 0.000000000000000000, -1.000000000000000000 ) ) ;
#17894 = ORIENTED_EDGE ( 'NONE', *, *, #18504, .T. ) ;
#17895 = DIRECTION ( 'NONE',  ( 0.000000000000000000, 0.000000000000000000, 1.000000000000000000 ) ) ;
#17896 = CIRCLE ( 'NONE', #1552, 7.500000000000007105 ) ;
#17897 = CARTESIAN_POINT ( 'NONE',  ( -92.20932192393669879, -118.3126747524536313, 47.79843924115901643 ) ) ;
#17898 = CIRCLE ( 'NONE', #895, 106.4288957539801146 ) ;
#17899 = CARTESIAN_POINT ( 'NONE',  ( -60.47951622432784546, -49.67518383744813804, 110.7293897666001214 ) ) ;
#17900 = DIRECTION ( 'NONE',  ( 0.5742676632334706710, 0.8186676071302499968, 0.000000000000000000 ) ) ;
#17901 = ORIENTED_EDGE ( 'NONE', *, *, #11514, .F. ) ;
#17902 = EDGE_CURVE ( 'NONE', #399, #9468, #12796, .T. ) ;
#17903 = CARTESIAN_POINT ( 'NONE',  ( -134.3888575020695271, -66.63121209263866263, 37.00842455669916831 ) ) ;
#17904 = DIRECTION ( 'NONE',  ( -0.8830229359480271656, -0.4693298356057563625, 0.000000000000000000 ) ) ;
#17905 = CARTESIAN_POINT ( 'NONE',  ( 10.99904278960855386, 0.5388563210141777970, 248.9926560891072143 ) ) ;
#17906 = CYLINDRICAL_SURFACE ( 'NONE', #18780, 15.91767397667354089 ) ;
#17907 = ORIENTED_EDGE ( 'NONE', *, *, #4681, .T. ) ;
#17908 = DIRECTION ( 'NONE',  ( -0.000000000000000000, -0.000000000000000000, 1.000000000000000000 ) ) ;
#17909 = CARTESIAN_POINT ( 'NONE',  ( 52.50000000000000711, 6.293851260911244545E-13, -115.0000000000000000 ) ) ;
#17910 = CARTESIAN_POINT ( 'NONE',  ( 83.87053960371954986, -124.3614079552663299, 1.354181719470851419 ) ) ;
#17911 = DIRECTION ( 'NONE',  ( -0.4338837391175662805, 0.9009688679024152602, 0.000000000000000000 ) ) ;
#17912 = AXIS2_PLACEMENT_3D ( 'NONE', #9885, #13141, #17681 ) ;
#17913 = ORIENTED_EDGE ( 'NONE', *, *, #6760, .F. ) ;
#17914 = CIRCLE ( 'NONE', #11035, 9.000000000000000000 ) ;
#17915 = CARTESIAN_POINT ( 'NONE',  ( -58.63718168490500204, -22.81000261549350228, 248.9926560891072143 ) ) ;
#17916 = CARTESIAN_POINT ( 'NONE',  ( 37.09555676056997697, -45.48770046196272432, 248.9926560891072143 ) ) ;
#17917 = EDGE_CURVE ( 'NONE', #5730, #1356, #6469, .T. ) ;
#17918 = ORIENTED_EDGE ( 'NONE', *, *, #8998, .T. ) ;
#17919 = EDGE_CURVE ( 'NONE', #9982, #13894, #14232, .T. ) ;
#17920 = ADVANCED_FACE ( 'NONE', ( #212 ), #19252, .F. ) ;
#17921 = ORIENTED_EDGE ( 'NONE', *, *, #13518, .F. ) ;
#17922 = ADVANCED_FACE ( 'NONE', ( #17421 ), #13654, .F. ) ;
#17923 = DIRECTION ( 'NONE',  ( -0.7818314824680221431, -0.6234898018587431423, -0.000000000000000000 ) ) ;
#17924 = ADVANCED_FACE ( 'NONE', ( #3295 ), #1856, .T. ) ;
#17925 = CARTESIAN_POINT ( 'NONE',  ( -109.9999999999983515, 275.0000000000000000, 77.50000000000000000 ) ) ;
#17926 = ORIENTED_EDGE ( 'NONE', *, *, #2154, .T. ) ;
#17927 = AXIS2_PLACEMENT_3D ( 'NONE', #18626, #197, #14214 ) ;
#17928 = CARTESIAN_POINT ( 'NONE',  ( 95.64660831655231732, -115.7365562161967745, 5.860842583562486219 ) ) ;
#17929 = CARTESIAN_POINT ( 'NONE',  ( -96.22303100966419720, -115.1714777947517803, 4.442967616989036195 ) ) ;
#17930 = VERTEX_POINT ( 'NONE', #12691 ) ;
#17931 = CIRCLE ( 'NONE', #16940, 62.91752772691707207 ) ;
#17932 = PLANE ( 'NONE',  #5559 ) ;
#17933 = FACE_OUTER_BOUND ( 'NONE', #2507, .T. ) ;
#17934 = FACE_OUTER_BOUND ( 'NONE', #16196, .T. ) ;
#17935 = LINE ( 'NONE', #3904, #10197 ) ;
#17936 = CARTESIAN_POINT ( 'NONE',  ( 45.46865632508072963, -40.28046525994365368, 283.5832628385307999 ) ) ;
#17937 = DIRECTION ( 'NONE',  ( -0.000000000000000000, -0.000000000000000000, 1.000000000000000000 ) ) ;
#17938 = LINE ( 'NONE', #1029, #94 ) ;
#17939 = VERTEX_POINT ( 'NONE', #9532 ) ;
#17940 = CARTESIAN_POINT ( 'NONE',  ( -8.938941455414985526, 60.08127757648384915, 293.5832628385307999 ) ) ;
#17941 = CARTESIAN_POINT ( 'NONE',  ( 57.92514141135453087, 18.28503710798567994, 283.5832628385307999 ) ) ;
#17942 = AXIS2_PLACEMENT_3D ( 'NONE', #10806, #13980, #2844 ) ;
#17943 = CIRCLE ( 'NONE', #13682, 62.91752772691707207 ) ;
#17944 = AXIS2_PLACEMENT_3D ( 'NONE', #8281, #11740, #18002 ) ;
#17945 = VECTOR ( 'NONE', #8851, 1000.000000000000114 ) ;
#17946 = ORIENTED_EDGE ( 'NONE', *, *, #15223, .F. ) ;
#17947 = EDGE_LOOP ( 'NONE', ( #765, #17216, #5565, #14548 ) ) ;
#17948 = EDGE_CURVE ( 'NONE', #8819, #11868, #278, .T. ) ;
#17949 = ORIENTED_EDGE ( 'NONE', *, *, #19008, .T. ) ;
#17950 = CARTESIAN_POINT ( 'NONE',  ( 52.50000000000000711, 6.293851260911244545E-13, -105.0000000000000142 ) ) ;
#17951 = AXIS2_PLACEMENT_3D ( 'NONE', #239, #6492, #12713 ) ;
#17952 = CARTESIAN_POINT ( 'NONE',  ( -44.07268132743698175, -38.78191089773056177, 132.4711112102474146 ) ) ;
#17953 = LINE ( 'NONE', #11401, #19240 ) ;
#17954 = CARTESIAN_POINT ( 'NONE',  ( -71.18887634719365565, -147.8252249328922687, 39.99999999999999289 ) ) ;
#17955 = FACE_OUTER_BOUND ( 'NONE', #19542, .T. ) ;
#17956 = VECTOR ( 'NONE', #9669, 1000.000000000000000 ) ;
#17957 = DIRECTION ( 'NONE',  ( -1.000000000000000000, 0.000000000000000000, 0.000000000000000000 ) ) ;
#17958 = CARTESIAN_POINT ( 'NONE',  ( -130.6671641404174977, -73.67117004794211255, -5.709326280083561578 ) ) ;
#17959 = LINE ( 'NONE', #19483, #3975 ) ;
#17960 = CYLINDRICAL_SURFACE ( 'NONE', #1007, 60.74260934110282051 ) ;
#17961 = DIRECTION ( 'NONE',  ( -0.000000000000000000, -1.000000000000000000, -0.000000000000000000 ) ) ;
#17962 = ORIENTED_EDGE ( 'NONE', *, *, #19303, .F. ) ;
#17963 =( REPRESENTATION_RELATIONSHIP ('NONE','NONE', #17382, #5472 ) REPRESENTATION_RELATIONSHIP_WITH_TRANSFORMATION ( #6869 )SHAPE_REPRESENTATION_RELATIONSHIP( ) );
#17964 = ORIENTED_EDGE ( 'NONE', *, *, #8045, .T. ) ;
#17965 = ORIENTED_EDGE ( 'NONE', *, *, #19303, .T. ) ;
#17966 = CIRCLE ( 'NONE', #13992, 7.500000000000020428 ) ;
#17967 = VECTOR ( 'NONE', #564, 1000.000000000000000 ) ;
#17968 = EDGE_LOOP ( 'NONE', ( #16754, #12305, #1093, #8637 ) ) ;
#17969 = EDGE_CURVE ( 'NONE', #18064, #16227, #11156, .T. ) ;
#17970 = CARTESIAN_POINT ( 'NONE',  ( 128.2779226595531270, 102.2982297021113141, 39.99999999999999289 ) ) ;
#17971 = ORIENTED_EDGE ( 'NONE', *, *, #15464, .F. ) ;
#17972 = DIRECTION ( 'NONE',  ( -0.8479630283625698706, 0.5300553768524376430, 0.000000000000000000 ) ) ;
#17973 = DIRECTION ( 'NONE',  ( 3.491481338843133355E-15, -1.000000000000000000, 0.000000000000000000 ) ) ;
#17974 = DIRECTION ( 'NONE',  ( 1.000000000000000000, 0.000000000000000000, 0.000000000000000000 ) ) ;
#17975 = VERTEX_POINT ( 'NONE', #6367 ) ;
#17976 = LINE ( 'NONE', #17776, #16840 ) ;
#17977 = CARTESIAN_POINT ( 'NONE',  ( -59.30716253403183202, 13.12726406102060217, 293.5832628385307999 ) ) ;
#17978 = VERTEX_POINT ( 'NONE', #18847 ) ;
#17979 = CARTESIAN_POINT ( 'NONE',  ( 40.32479851956816930, -67.08601213326551260, 132.4711112102474146 ) ) ;
#17980 = EDGE_CURVE ( 'NONE', #934, #1238, #19055, .T. ) ;
#17981 = CARTESIAN_POINT ( 'NONE',  ( -22.30005961346265408, -56.50329132715937419, 293.5832628385307999 ) ) ;
#17982 = DIRECTION ( 'NONE',  ( 1.000000000000000000, 0.000000000000000000, 0.000000000000000000 ) ) ;
#17983 = CIRCLE ( 'NONE', #18971, 60.74260934110282051 ) ;
#17984 = CARTESIAN_POINT ( 'NONE',  ( 0.000000000000000000, 0.000000000000000000, -49.99999999999999289 ) ) ;
#17985 = CARTESIAN_POINT ( 'NONE',  ( 150.0000000000000284, 1.836970198721029747E-14, 49.99999999999999289 ) ) ;
#17986 = DIRECTION ( 'NONE',  ( 0.5000000000000101030, -0.8660254037844328234, 0.000000000000000000 ) ) ;
#17987 = EDGE_LOOP ( 'NONE', ( #6518, #19030, #7212, #1396 ) ) ;
#17988 = DIRECTION ( 'NONE',  ( -0.000000000000000000, -0.000000000000000000, 1.000000000000000000 ) ) ;
#17989 = ORIENTED_EDGE ( 'NONE', *, *, #6788, .F. ) ;
#17990 = ORIENTED_EDGE ( 'NONE', *, *, #1365, .F. ) ;
#17991 = EDGE_CURVE ( 'NONE', #8910, #5730, #8192, .T. ) ;
#17992 = CARTESIAN_POINT ( 'NONE',  ( -113.3514208120935933, -17.29894464209964866, 39.88498244535624337 ) ) ;
#17993 = ORIENTED_EDGE ( 'NONE', *, *, #11030, .T. ) ;
#17994 = AXIS2_PLACEMENT_3D ( 'NONE', #18003, #9923, #2159 ) ;
#17995 = FACE_OUTER_BOUND ( 'NONE', #15005, .T. ) ;
#17996 = DIRECTION ( 'NONE',  ( -0.9396926207859104263, 0.3420201433256630508, 0.000000000000000000 ) ) ;
#17997 = DIRECTION ( 'NONE',  ( 0.7660444431189749048, 0.6427876096865430267, 0.000000000000000000 ) ) ;
#17998 = DIRECTION ( 'NONE',  ( 0.000000000000000000, 0.000000000000000000, 1.000000000000000000 ) ) ;
#17999 = ORIENTED_EDGE ( 'NONE', *, *, #8016, .T. ) ;
#18000 = ADVANCED_FACE ( 'NONE', ( #17520 ), #17318, .T. ) ;
#18001 = CARTESIAN_POINT ( 'NONE',  ( -107.4999999999999858, -118.5063289449133777, -10.00000000000000000 ) ) ;
#18002 = DIRECTION ( 'NONE',  ( 1.000000000000000000, 0.000000000000000000, 0.000000000000000000 ) ) ;
#18003 = CARTESIAN_POINT ( 'NONE',  ( -63.98537287693041264, 94.20918150411493741, 14.88498244535589876 ) ) ;
#18004 = EDGE_CURVE ( 'NONE', #3096, #10368, #2067, .T. ) ;
#18005 = CARTESIAN_POINT ( 'NONE',  ( -159.9599531637108782, -36.50981547337168109, 49.99999999999999289 ) ) ;
#18006 = AXIS2_PLACEMENT_3D ( 'NONE', #8356, #9794, #5005 ) ;
#18007 = ORIENTED_EDGE ( 'NONE', *, *, #11610, .T. ) ;
#18008 = DIRECTION ( 'NONE',  ( -0.1390141521205912334, 0.9902903945359629034, 0.000000000000000000 ) ) ;
#18009 = CARTESIAN_POINT ( 'NONE',  ( 93.79892245610579948, -117.0565612855932329, -8.571526395727955716 ) ) ;
#18010 = DIRECTION ( 'NONE',  ( 0.000000000000000000, -0.000000000000000000, 1.000000000000000000 ) ) ;
#18011 = ORIENTED_EDGE ( 'NONE', *, *, #14038, .T. ) ;
#18012 = CARTESIAN_POINT ( 'NONE',  ( -100.7812499999999716, -111.0996833858562809, 49.99999999999999289 ) ) ;
#18013 = CARTESIAN_POINT ( 'NONE',  ( 61.81362617575100415, -11.73417718768069840, 248.9926560891072143 ) ) ;
#18014 = VERTEX_POINT ( 'NONE', #15876 ) ;
#18015 = EDGE_LOOP ( 'NONE', ( #15953, #10681, #167, #839 ) ) ;
#18016 = AXIS2_PLACEMENT_3D ( 'NONE', #550, #7906, #1679 ) ;
#18017 = EDGE_CURVE ( 'NONE', #4108, #7679, #2556, .T. ) ;
#18018 = DIRECTION ( 'NONE',  ( 0.3420201433256790380, -0.9396926207859046531, 0.000000000000000000 ) ) ;
#18019 = AXIS2_PLACEMENT_3D ( 'NONE', #15063, #1042, #7291 ) ;
#18020 = FACE_OUTER_BOUND ( 'NONE', #5013, .T. ) ;
#18021 = ORIENTED_EDGE ( 'NONE', *, *, #8997, .T. ) ;
#18022 = AXIS2_PLACEMENT_3D ( 'NONE', #18752, #10956, #17217 ) ;
#18023 = DIRECTION ( 'NONE',  ( 0.7660444431189771253, 0.6427876096865405842, 0.000000000000000000 ) ) ;
#18024 = CARTESIAN_POINT ( 'NONE',  ( -85.70335357680858124, -123.1056148428088335, -1.893379215449441988 ) ) ;
#18025 = EDGE_CURVE ( 'NONE', #13281, #3444, #5040, .T. ) ;
#18026 = ADVANCED_FACE ( 'NONE', ( #11365 ), #6864, .T. ) ;
#18027 = DIRECTION ( 'NONE',  ( -6.982962677686266711E-15, 0.000000000000000000, -1.000000000000000000 ) ) ;
#18028 =( BOUNDED_CURVE ( )  B_SPLINE_CURVE ( 3, ( #14512, #12871, #14103, #11029 ),
 .UNSPECIFIED., .F., .F. ) 
 B_SPLINE_CURVE_WITH_KNOTS ( ( 4, 4 ),
 ( 3.141592653589794004, 4.712388980384689674 ),
 .UNSPECIFIED. ) 
 CURVE ( )  GEOMETRIC_REPRESENTATION_ITEM ( )  RATIONAL_B_SPLINE_CURVE ( ( 1.000000000000000000, 0.8047378541243652705, 0.8047378541243652705, 1.000000000000000000 ) ) 
 REPRESENTATION_ITEM ( '' )  );
#18029 = LINE ( 'NONE', #16494, #17139 ) ;
#18030 = DIRECTION ( 'NONE',  ( 0.000000000000000000, 0.000000000000000000, 1.000000000000000000 ) ) ;
#18031 = DIRECTION ( 'NONE',  ( 0.000000000000000000, 0.000000000000000000, 1.000000000000000000 ) ) ;
#18032 = DIRECTION ( 'NONE',  ( -6.982962677686266711E-15, 0.000000000000000000, -1.000000000000000000 ) ) ;
#18033 = CARTESIAN_POINT ( 'NONE',  ( 78.26059000578310076, 1.379293853802574743, 112.7772637782949516 ) ) ;
#18034 = EDGE_LOOP ( 'NONE', ( #6477, #11690, #20171, #9073 ) ) ;
#18035 = CARTESIAN_POINT ( 'NONE',  ( 14.85701326357409968, 22.71800723006099432, 14.88498244535534809 ) ) ;
#18036 = LINE ( 'NONE', #11969, #14150 ) ;
#18037 = ORIENTED_EDGE ( 'NONE', *, *, #19369, .F. ) ;
#18038 = EDGE_CURVE ( 'NONE', #17975, #6230, #10078, .T. ) ;
#18039 = VECTOR ( 'NONE', #16616, 999.9999999999998863 ) ;
#18040 = ORIENTED_EDGE ( 'NONE', *, *, #13228, .F. ) ;
#18041 = LINE ( 'NONE', #16508, #4798 ) ;
#18042 = ORIENTED_EDGE ( 'NONE', *, *, #6159, .F. ) ;
#18043 = CARTESIAN_POINT ( 'NONE',  ( 134.1070788506805513, -77.29467090009929109, 3.900409095995342135 ) ) ;
#18044 = DIRECTION ( 'NONE',  ( 0.8660254037844449249, -0.4999999999999888978, 0.000000000000000000 ) ) ;
#18045 = CARTESIAN_POINT ( 'NONE',  ( 60.74260934110282051, 0.000000000000000000, 283.5832628385307999 ) ) ;
#18046 = EDGE_CURVE ( 'NONE', #399, #4738, #3868, .T. ) ;
#18047 = DIRECTION ( 'NONE',  ( 0.000000000000000000, 0.000000000000000000, 1.000000000000000000 ) ) ;
#18048 = CARTESIAN_POINT ( 'NONE',  ( 110.0000000000000142, 0.000000000000000000, -39.99999999999999289 ) ) ;
#18049 = LINE ( 'NONE', #16219, #10968 ) ;
#18050 = CARTESIAN_POINT ( 'NONE',  ( 132.3553460543369908, -70.70324312373998055, 4.525982478036794099 ) ) ;
#18051 = AXIS2_PLACEMENT_3D ( 'NONE', #10564, #14157, #12509 ) ;
#18052 = AXIS2_PLACEMENT_3D ( 'NONE', #10530, #7369, #4406 ) ;
#18053 = DIRECTION ( 'NONE',  ( 6.982962677686266711E-15, -0.000000000000000000, 1.000000000000000000 ) ) ;
#18054 = CARTESIAN_POINT ( 'NONE',  ( 67.36461649554532016, -39.84224160888924615, 110.9660488491357455 ) ) ;
#18055 = CARTESIAN_POINT ( 'NONE',  ( 0.000000000000000000, 0.000000000000000000, 50.00000000000000000 ) ) ;
#18056 = EDGE_CURVE ( 'NONE', #18133, #2863, #4525, .T. ) ;
#18057 = ORIENTED_EDGE ( 'NONE', *, *, #1789, .F. ) ;
#18058 = AXIS2_PLACEMENT_3D ( 'NONE', #14848, #16499, #5748 ) ;
#18059 = CIRCLE ( 'NONE', #17418, 140.0000000000000000 ) ;
#18060 = ORIENTED_EDGE ( 'NONE', *, *, #8222, .F. ) ;
#18061 = VERTEX_POINT ( 'NONE', #13088 ) ;
#18062 = ORIENTED_EDGE ( 'NONE', *, *, #7352, .T. ) ;
#18063 = CIRCLE ( 'NONE', #15448, 60.74260934110282051 ) ;
#18064 = VERTEX_POINT ( 'NONE', #17915 ) ;
#18065 = CARTESIAN_POINT ( 'NONE',  ( -57.92514141135452377, -18.28503710798565152, 283.5832628385307999 ) ) ;
#18066 = CARTESIAN_POINT ( 'NONE',  ( -13.12726406102078336, -59.30716253403180360, 283.5832628385307999 ) ) ;
#18067 = ORIENTED_EDGE ( 'NONE', *, *, #13785, .F. ) ;
#18068 = AXIS2_PLACEMENT_3D ( 'NONE', #5602, #11819, #18085 ) ;
#18069 = PLANE ( 'NONE',  #16529 ) ;
#18070 = DIRECTION ( 'NONE',  ( 0.000000000000000000, 0.000000000000000000, 1.000000000000000000 ) ) ;
#18071 = VERTEX_POINT ( 'NONE', #16180 ) ;
#18072 = DIRECTION ( 'NONE',  ( 1.000000000000000000, 0.000000000000000000, 0.000000000000000000 ) ) ;
#18073 = LINE ( 'NONE', #16542, #557 ) ;
#18074 = CARTESIAN_POINT ( 'NONE',  ( 20.74471755083603597, -59.39925916207552348, 248.9926560891072143 ) ) ;
#18075 = LINE ( 'NONE', #8754, #45 ) ;
#18076 = VECTOR ( 'NONE', #17988, 1000.000000000000000 ) ;
#18077 = COLOUR_RGB ( '', 0.72549020, 0.75294118, 0.79215686) ;
#18078 = CARTESIAN_POINT ( 'NONE',  ( 133.3574802752771404, -81.67441013337949585, 38.22103175428581778 ) ) ;
#18079 = DIRECTION ( 'NONE',  ( 0.000000000000000000, 0.000000000000000000, 1.000000000000000000 ) ) ;
#18080 = ORIENTED_EDGE ( 'NONE', *, *, #19887, .F. ) ;
#18081 = CARTESIAN_POINT ( 'NONE',  ( -60.68567895461851691, 2.629250726500500956, 293.5832628385307999 ) ) ;
#18082 = ORIENTED_EDGE ( 'NONE', *, *, #4911, .T. ) ;
#18083 = AXIS2_PLACEMENT_3D ( 'NONE', #5865, #4423, #16805 ) ;
#18084 = ORIENTED_EDGE ( 'NONE', *, *, #11209, .F. ) ;
#18085 = DIRECTION ( 'NONE',  ( 0.000000000000000000, 0.000000000000000000, 1.000000000000000000 ) ) ;
#18086 = CIRCLE ( 'NONE', #2420, 62.91752772691707207 ) ;
#18087 = ORIENTED_EDGE ( 'NONE', *, *, #5757, .T. ) ;
#18088 = EDGE_LOOP ( 'NONE', ( #17503, #15443, #263 ) ) ;
#18089 = DIRECTION ( 'NONE',  ( -0.000000000000000000, -0.000000000000000000, 1.000000000000000000 ) ) ;
#18090 = CARTESIAN_POINT ( 'NONE',  ( -93.26156191356919578, -117.4850166029420677, 48.33165481139338482 ) ) ;
#18091 = CARTESIAN_POINT ( 'NONE',  ( 78.26059000578312919, -0.8220851292427139301, 132.4711112102474146 ) ) ;
#18092 = CARTESIAN_POINT ( 'NONE',  ( -117.2142335457655520, -12.13581325405623268, 14.88498244535627002 ) ) ;
#18093 = VERTEX_POINT ( 'NONE', #18012 ) ;
#18094 = CARTESIAN_POINT ( 'NONE',  ( -1.678175111358159333, -5.485913980968224912, 293.5832628385307999 ) ) ;
#18095 = DIRECTION ( 'NONE',  ( -0.000000000000000000, -0.000000000000000000, 1.000000000000000000 ) ) ;
#18096 = EDGE_CURVE ( 'NONE', #15899, #18157, #10220, .T. ) ;
#18097 = LINE ( 'NONE', #2932, #13723 ) ;
#18098 = DIRECTION ( 'NONE',  ( -0.9009688679024212554, 0.4338837391175534575, 0.000000000000000000 ) ) ;
#18099 = ORIENTED_EDGE ( 'NONE', *, *, #4270, .T. ) ;
#18100 = STYLED_ITEM ( 'NONE', ( #18292 ), #1084 ) ;
#18101 = DIRECTION ( 'NONE',  ( -0.2080686897406911207, -0.9781142164131917394, 0.000000000000000000 ) ) ;
#18102 = CARTESIAN_POINT ( 'NONE',  ( 82.33470881469955316, -125.3834122142801277, 6.398087192529462897 ) ) ;
#18103 = CARTESIAN_POINT ( 'NONE',  ( -22.81000261549329267, 58.63718168490507310, 248.9926560891072143 ) ) ;
#18104 = ORIENTED_EDGE ( 'NONE', *, *, #1990, .T. ) ;
#18105 = CARTESIAN_POINT ( 'NONE',  ( -148.9554720520392834, -17.67108784863415138, 49.99999999999999289 ) ) ;
#18106 = CARTESIAN_POINT ( 'NONE',  ( 0.000000000000000000, 0.000000000000000000, 283.5832628385307999 ) ) ;
#18107 = VERTEX_POINT ( 'NONE', #14636 ) ;
#18108 = ORIENTED_EDGE ( 'NONE', *, *, #6, .F. ) ;
#18109 = EDGE_CURVE ( 'NONE', #3934, #14411, #14732, .T. ) ;
#18110 = EDGE_CURVE ( 'NONE', #16849, #3604, #17931, .T. ) ;
#18111 = VECTOR ( 'NONE', #15868, 1000.000000000000000 ) ;
#18112 = ADVANCED_FACE ( 'NONE', ( #2358 ), #16285, .F. ) ;
#18113 = LINE ( 'NONE', #4087, #19239 ) ;
#18114 = DIRECTION ( 'NONE',  ( 0.4999999999999916178, -0.8660254037844435926, -3.228294802704586902E-15 ) ) ;
#18115 = VECTOR ( 'NONE', #19378, 1000.000000000000000 ) ;
#18116 = ORIENTED_EDGE ( 'NONE', *, *, #17671, .F. ) ;
#18117 = LINE ( 'NONE', #1119, #19471 ) ;
#18118 = DIRECTION ( 'NONE',  ( 1.000000000000000000, 0.000000000000000000, 0.000000000000000000 ) ) ;
#18119 = EDGE_CURVE ( 'NONE', #1551, #10080, #621, .T. ) ;
#18120 = CARTESIAN_POINT ( 'NONE',  ( -82.61717615486091404, -125.1974987762635152, 5.026310667705078394 ) ) ;
#18121 = CARTESIAN_POINT ( 'NONE',  ( -110.0000000000000142, 1.530808498934191876E-14, -39.99999999999999289 ) ) ;
#18122 = CARTESIAN_POINT ( 'NONE',  ( 54.67896814532641514, 21.36933070621782349, 132.4711112102474146 ) ) ;
#18123 = CIRCLE ( 'NONE', #17819, 112.8770930172170210 ) ;
#18124 = LINE ( 'NONE', #13201, #8141 ) ;
#18125 = CARTESIAN_POINT ( 'NONE',  ( 57.65577537092158877, -11.00103590902891249, 248.9926560891072143 ) ) ;
#18126 = ORIENTED_EDGE ( 'NONE', *, *, #9905, .T. ) ;
#18127 = DIRECTION ( 'NONE',  ( 0.1390141521205912056, -0.9902903945359629034, 0.000000000000000000 ) ) ;
#18128 = DIRECTION ( 'NONE',  ( 1.000000000000000000, 0.000000000000000000, 0.000000000000000000 ) ) ;
#18129 = ORIENTED_EDGE ( 'NONE', *, *, #16410, .T. ) ;
#18130 = ORIENTED_EDGE ( 'NONE', *, *, #12105, .F. ) ;
#18131 =( LENGTH_UNIT ( ) NAMED_UNIT ( * ) SI_UNIT ( .MILLI., .METRE. ) );
#18132 = EDGE_CURVE ( 'NONE', #15095, #6267, #4184, .T. ) ;
#18133 = VERTEX_POINT ( 'NONE', #2457 ) ;
#18134 = EDGE_CURVE ( 'NONE', #2090, #9172, #8117, .T. ) ;
#18135 = DIRECTION ( 'NONE',  ( 0.000000000000000000, 0.000000000000000000, 1.000000000000000000 ) ) ;
#18136 = EDGE_LOOP ( 'NONE', ( #11798, #12667, #19912, #12702 ) ) ;
#18137 = CARTESIAN_POINT ( 'NONE',  ( 134.3956174703911017, -75.35551001548425631, 5.362548286559334798 ) ) ;
#18138 = CARTESIAN_POINT ( 'NONE',  ( 41.02350267428969488, 44.79940644582669051, 293.5832628385307999 ) ) ;
#18139 = CARTESIAN_POINT ( 'NONE',  ( 0.000000000000000000, 0.000000000000000000, 283.5832628385307999 ) ) ;
#18140 = CARTESIAN_POINT ( 'NONE',  ( 138.2024300533213932, 89.85329105948596862, 49.99999999999999289 ) ) ;
#18141 = CARTESIAN_POINT ( 'NONE',  ( 4.189777606611760026E-13, -60.00000000000000000, -105.0000000000000142 ) ) ;
#18142 = ORIENTED_EDGE ( 'NONE', *, *, #4601, .T. ) ;
#18143 = CYLINDRICAL_SURFACE ( 'NONE', #20221, 60.74260934110282051 ) ;
#18144 = DIRECTION ( 'NONE',  ( 1.000000000000000000, 0.000000000000000000, 0.000000000000000000 ) ) ;
#18145 = ADVANCED_FACE ( 'NONE', ( #5726 ), #10132, .T. ) ;
#18146 = CARTESIAN_POINT ( 'NONE',  ( 51.23821591265094355, 28.63313560863489471, 248.9926560891072143 ) ) ;
#18147 = DIRECTION ( 'NONE',  ( -0.000000000000000000, -0.000000000000000000, 1.000000000000000000 ) ) ;
#18148 = VECTOR ( 'NONE', #200, 1000.000000000000000 ) ;
#18149 = FACE_OUTER_BOUND ( 'NONE', #5768, .T. ) ;
#18150 = DIRECTION ( 'NONE',  ( -0.7818314824680222541, -0.6234898018587428092, 0.000000000000000000 ) ) ;
#18151 = ORIENTED_EDGE ( 'NONE', *, *, #14769, .T. ) ;
#18152 = VERTEX_POINT ( 'NONE', #19730 ) ;
#18153 = ORIENTED_EDGE ( 'NONE', *, *, #9531, .T. ) ;
#18154 = EDGE_CURVE ( 'NONE', #1847, #4859, #1010, .T. ) ;
#18155 = EDGE_CURVE ( 'NONE', #16933, #870, #5186, .T. ) ;
#18156 = ORIENTED_EDGE ( 'NONE', *, *, #8619, .F. ) ;
#18157 = VERTEX_POINT ( 'NONE', #5624 ) ;
#18158 = DIRECTION ( 'NONE',  ( 0.9396926207859112035, 0.3420201433256609969, -6.456589605409174593E-15 ) ) ;
#18159 = EDGE_CURVE ( 'NONE', #6447, #6551, #14926, .T. ) ;
#18160 = CIRCLE ( 'NONE', #14533, 60.74260934110282051 ) ;
#18161 = CARTESIAN_POINT ( 'NONE',  ( 56.50329132715945235, -22.30005961346246579, 293.5832628385307999 ) ) ;
#18162 = CARTESIAN_POINT ( 'NONE',  ( 44.79787735033391272, -41.02212542604627288, 283.5832628385307999 ) ) ;
#18163 = ORIENTED_EDGE ( 'NONE', *, *, #4898, .T. ) ;
#18164 = CARTESIAN_POINT ( 'NONE',  ( 0.07661102881317166657, -8.673996836102537245, 2.976196775178697962 ) ) ;
#18165 = DIRECTION ( 'NONE',  ( 1.000000000000000000, 0.000000000000000000, 0.000000000000000000 ) ) ;
#18166 = EDGE_LOOP ( 'NONE', ( #4415, #12802 ) ) ;
#18167 = CARTESIAN_POINT ( 'NONE',  ( -45.46712722958807973, 40.27908801170008957, 283.5832628385307999 ) ) ;
#18168 = LINE ( 'NONE', #8852, #2504 ) ;
#18169 = CARTESIAN_POINT ( 'NONE',  ( -134.2328839869800277, -76.48032294689467392, 4.418921395648128581 ) ) ;
#18170 = CARTESIAN_POINT ( 'NONE',  ( 5.111158570922285982, -2.605298826210321383, 293.5832628385307999 ) ) ;
#18171 = AXIS2_PLACEMENT_3D ( 'NONE', #7314, #15397, #12423 ) ;
#18172 = VECTOR ( 'NONE', #9226, 1000.000000000000000 ) ;
#18173 = CARTESIAN_POINT ( 'NONE',  ( 60.47951622432751151, 49.67518383744852883, 248.9926560891072143 ) ) ;
#18174 = DIRECTION ( 'NONE',  ( 1.000000000000000000, 0.000000000000000000, 0.000000000000000000 ) ) ;
#18175 = ORIENTED_EDGE ( 'NONE', *, *, #17268, .T. ) ;
#18176 = B_SPLINE_CURVE_WITH_KNOTS ( 'NONE', 3,
 ( #8046, #6327, #14297, #3348, #11322, #4899, #8247, #11112, #3150, #19207, #7840, #17375, #9385, #4790, #9785, #15933, #12753, #12546, #19013, #7942, #15833, #15628, #1616, #9587 ),
 .UNSPECIFIED., .F., .F.,
 ( 4, 2, 2, 2, 2, 2, 2, 2, 2, 2, 2, 4 ),
 ( 0.000000000000000000, 0.005718059174761352254, 0.008577088762142017972, 0.01143611834952268543, 0.01286563314321301742, 0.01429514793690335114, 0.01715417752428397696, 0.01858369231797427773, 0.02001320711166457503, 0.02072796450850974623, 0.02144272190535492090, 0.02287223669904525289 ),
 .UNSPECIFIED. ) ;
#18177 = CIRCLE ( 'NONE', #1181, 7.500000000000020428 ) ;
#18178 = CARTESIAN_POINT ( 'NONE',  ( 60.00000000000000711, 6.284666409917639535E-13, -105.0000000000000142 ) ) ;
#18179 = ORIENTED_EDGE ( 'NONE', *, *, #705, .T. ) ;
#18180 = EDGE_LOOP ( 'NONE', ( #8840, #14239, #324, #10418 ) ) ;
#18181 = DIRECTION ( 'NONE',  ( 1.000000000000000000, 0.000000000000000000, 0.000000000000000000 ) ) ;
#18182 = ORIENTED_EDGE ( 'NONE', *, *, #10019, .T. ) ;
#18183 = ORIENTED_EDGE ( 'NONE', *, *, #4401, .T. ) ;
#18184 = VECTOR ( 'NONE', #9594, 1000.000000000000000 ) ;
#18185 = CARTESIAN_POINT ( 'NONE',  ( -17.50000000000001066, 2.143131898507869431E-15, 4.999999999999948486 ) ) ;
#18186 = VECTOR ( 'NONE', #2669, 1000.000000000000227 ) ;
#18187 = SURFACE_SIDE_STYLE ('',( #12337 ) ) ;
#18188 = CARTESIAN_POINT ( 'NONE',  ( -13.12769224524071277, -59.30917539369501412, 293.5832628385307999 ) ) ;
#18189 = CARTESIAN_POINT ( 'NONE',  ( 15.91767397667355510, 149.1530343478547138, 49.99999999999999289 ) ) ;
#18190 = LINE ( 'NONE', #5924, #2454 ) ;
#18191 = EDGE_LOOP ( 'NONE', ( #19566, #9939, #8526, #17166 ) ) ;
#18192 = AXIS2_PLACEMENT_3D ( 'NONE', #7569, #1445, #15455 ) ;
#18193 = DIRECTION ( 'NONE',  ( 0.000000000000000000, 0.000000000000000000, -1.000000000000000000 ) ) ;
#18194 = LINE ( 'NONE', #15020, #8116 ) ;
#18195 = PLANE ( 'NONE',  #17497 ) ;
#18196 = ORIENTED_EDGE ( 'NONE', *, *, #7466, .T. ) ;
#18197 = CARTESIAN_POINT ( 'NONE',  ( 59.58067424803626011, -20.21777810286696564, 293.5832628385307999 ) ) ;
#18198 = LINE ( 'NONE', #16972, #670 ) ;
#18199 = FACE_OUTER_BOUND ( 'NONE', #18136, .T. ) ;
#18200 = ORIENTED_EDGE ( 'NONE', *, *, #592, .F. ) ;
#18201 = CARTESIAN_POINT ( 'NONE',  ( 0.000000000000000000, 0.000000000000000000, 283.5832628385307999 ) ) ;
#18202 = DIRECTION ( 'NONE',  ( 0.000000000000000000, 0.000000000000000000, 1.000000000000000000 ) ) ;
#18203 = ORIENTED_EDGE ( 'NONE', *, *, #10096, .T. ) ;
#18204 = ORIENTED_EDGE ( 'NONE', *, *, #12850, .T. ) ;
#18205 = CARTESIAN_POINT ( 'NONE',  ( 57.92709869106709419, 18.28567271940532990, 293.5832628385307999 ) ) ;
#18206 = AXIS2_PLACEMENT_3D ( 'NONE', #9082, #10715, #2959 ) ;
#18207 = ORIENTED_EDGE ( 'NONE', *, *, #5226, .T. ) ;
#18208 = ADVANCED_FACE ( 'NONE', ( #2557 ), #814, .T. ) ;
#18209 = CARTESIAN_POINT ( 'NONE',  ( 81.66698895276879000, 79.37254397626031732, 14.88498244535488269 ) ) ;
#18210 = CARTESIAN_POINT ( 'NONE',  ( 30.09424155357379504, 27.05260723904837761, 248.9926560891072143 ) ) ;
#18211 = VERTEX_POINT ( 'NONE', #15030 ) ;
#18212 = CARTESIAN_POINT ( 'NONE',  ( 97.52493780047066707, -113.9981091059116096, 2.471315604452407388 ) ) ;
#18213 = CARTESIAN_POINT ( 'NONE',  ( -76.83212392882499842, -14.94814811854936210, 112.0427633081291816 ) ) ;
#18214 =( REPRESENTATION_RELATIONSHIP ('NONE','NONE', #17382, #15821 ) REPRESENTATION_RELATIONSHIP_WITH_TRANSFORMATION ( #16384 )SHAPE_REPRESENTATION_RELATIONSHIP( ) );
#18215 = CIRCLE ( 'NONE', #245, 15.91767397667354800 ) ;
#18216 = DIRECTION ( 'NONE',  ( 0.9396926207859092051, -0.3420201433256662704, 0.000000000000000000 ) ) ;
#18217 = CARTESIAN_POINT ( 'NONE',  ( -110.0000000000000142, 0.000000000000000000, -29.99999999999998224 ) ) ;
#18218 = AXIS2_PLACEMENT_3D ( 'NONE', #13404, #10437, #5751 ) ;
#18219 = ADVANCED_FACE ( 'NONE', ( #13689, #18509, #9088, #7656, #2860, #7452, #10416, #19933, #5938, #15329, #15224 ), #12359, .T. ) ;
#18220 = DIRECTION ( 'NONE',  ( 0.000000000000000000, 0.5000000000000009992, -0.8660254037844380415 ) ) ;
#18221 = DIRECTION ( 'NONE',  ( -0.6234898018587431423, 0.7818314824680221431, 0.000000000000000000 ) ) ;
#18222 = CARTESIAN_POINT ( 'NONE',  ( 0.000000000000000000, 0.000000000000000000, 132.4711112102474146 ) ) ;
#18223 = PLANE ( 'NONE',  #18058 ) ;
#18224 = ORIENTED_EDGE ( 'NONE', *, *, #19859, .F. ) ;
#18225 = EDGE_CURVE ( 'NONE', #1059, #10466, #10511, .T. ) ;
#18226 = LINE ( 'NONE', #16502, #3206 ) ;
#18227 = DIRECTION ( 'NONE',  ( -0.9511061040868794558, -0.3088643371590157338, 0.000000000000000000 ) ) ;
#18228 = VERTEX_POINT ( 'NONE', #4386 ) ;
#18229 = VERTEX_POINT ( 'NONE', #7554 ) ;
#18230 = VERTEX_POINT ( 'NONE', #10615 ) ;
#18231 = EDGE_CURVE ( 'NONE', #14483, #18743, #12358, .T. ) ;
#18232 = AXIS2_PLACEMENT_3D ( 'NONE', #16869, #16673, #8882 ) ;
#18233 = LINE ( 'NONE', #12947, #13260 ) ;
#18234 = EDGE_LOOP ( 'NONE', ( #19003, #2161, #16429, #2588 ) ) ;
#18235 = CARTESIAN_POINT ( 'NONE',  ( 131.2498835542438655, -90.93927553429132615, -1.384616524445031067E-15 ) ) ;
#18236 = DIRECTION ( 'NONE',  ( 6.982962677686266711E-15, -0.000000000000000000, 1.000000000000000000 ) ) ;
#18237 = CARTESIAN_POINT ( 'NONE',  ( -29.99999999999887379, 265.0000000000000000, 4.999999999999158007 ) ) ;
#18238 = CARTESIAN_POINT ( 'NONE',  ( -62.91215678473958661, 0.8220851292433132285, 132.4711112102474146 ) ) ;
#18239 = ORIENTED_EDGE ( 'NONE', *, *, #8275, .T. ) ;
#18240 = DIRECTION ( 'NONE',  ( 0.9848077530122069101, 0.1736481776669374644, 0.000000000000000000 ) ) ;
#18241 = CARTESIAN_POINT ( 'NONE',  ( -130.5346569919981334, -73.99347627471406952, 1.284038776032530249 ) ) ;
#18242 = EDGE_CURVE ( 'NONE', #11033, #13701, #913, .T. ) ;
#18243 = CARTESIAN_POINT ( 'NONE',  ( 130.9868171408399462, -91.88282611735540684, 0.000000000000000000 ) ) ;
#18244 = AXIS2_PLACEMENT_3D ( 'NONE', #4791, #6225, #13776 ) ;
#18245 = CARTESIAN_POINT ( 'NONE',  ( -176.7850001792984926, -190.0000000000000284, 6.572490470375933036 ) ) ;
#18246 = CARTESIAN_POINT ( 'NONE',  ( -148.9554720520393118, -17.67108784863417270, 49.99999999999999289 ) ) ;
#18247 = CIRCLE ( 'NONE', #9085, 7.500000000000007105 ) ;
#18248 = CYLINDRICAL_SURFACE ( 'NONE', #12897, 7.500000000000000000 ) ;
#18249 = VECTOR ( 'NONE', #4907, 1000.000000000000227 ) ;
#18250 = ORIENTED_EDGE ( 'NONE', *, *, #13252, .F. ) ;
#18251 = ADVANCED_FACE ( 'NONE', ( #2660 ), #15127, .F. ) ;
#18252 = AXIS2_PLACEMENT_3D ( 'NONE', #19504, #11806, #687 ) ;
#18253 = DIRECTION ( 'NONE',  ( 1.000000000000000000, 0.000000000000000000, -0.000000000000000000 ) ) ;
#18254 = EDGE_LOOP ( 'NONE', ( #12484, #6008, #15186, #1760, #2024, #11891 ) ) ;
#18255 = EDGE_LOOP ( 'NONE', ( #11973, #14029, #2842, #16577 ) ) ;
#18256 = VERTEX_POINT ( 'NONE', #13581 ) ;
#18257 = EDGE_CURVE ( 'NONE', #4516, #10035, #20137, .T. ) ;
#18258 = ORIENTED_EDGE ( 'NONE', *, *, #1752, .T. ) ;
#18259 = VECTOR ( 'NONE', #2880, 1000.000000000000000 ) ;
#18260 = AXIS2_PLACEMENT_3D ( 'NONE', #15640, #7853, #18819 ) ;
#18261 = CARTESIAN_POINT ( 'NONE',  ( -138.3191304882901420, -25.24048809540655469, 25.56945045193375776 ) ) ;
#18262 = CIRCLE ( 'NONE', #10736, 17.50000000000001066 ) ;
#18263 = CARTESIAN_POINT ( 'NONE',  ( 167.4599531637113330, -36.50981547336952104, 60.00000000000000000 ) ) ;
#18264 = DIRECTION ( 'NONE',  ( 0.000000000000000000, 0.000000000000000000, 1.000000000000000000 ) ) ;
#18265 = ORIENTED_EDGE ( 'NONE', *, *, #9369, .F. ) ;
#18266 = CARTESIAN_POINT ( 'NONE',  ( 1.396592535537252080E-14, 0.000000000000000000, 127.7817459305202448 ) ) ;
#18267 = CARTESIAN_POINT ( 'NONE',  ( 56.12662799072089115, -23.22641211976269915, 293.5832628385307999 ) ) ;
#18268 = ORIENTED_EDGE ( 'NONE', *, *, #9978, .T. ) ;
#18269 = DIRECTION ( 'NONE',  ( 0.000000000000000000, 0.000000000000000000, 1.000000000000000000 ) ) ;
#18270 = CARTESIAN_POINT ( 'NONE',  ( -60.47951622432783125, -49.67518383744813804, 132.4711112102474146 ) ) ;
#18271 = CARTESIAN_POINT ( 'NONE',  ( -133.6066233479225787, -80.29760051435191315, 2.337471363756875586 ) ) ;
#18272 = ADVANCED_FACE ( 'NONE', ( #19829 ), #7353, .F. ) ;
#18273 = EDGE_CURVE ( 'NONE', #1270, #12482, #2761, .T. ) ;
#18274 = DIRECTION ( 'NONE',  ( -0.4338837391175523472, -0.9009688679024219216, 0.000000000000000000 ) ) ;
#18275 = EDGE_CURVE ( 'NONE', #13097, #16122, #14651, .T. ) ;
#18276 = ADVANCED_FACE ( 'NONE', ( #1428 ), #12046, .F. ) ;
#18277 = EDGE_CURVE ( 'NONE', #4586, #6529, #5842, .T. ) ;
#18278 = DIRECTION ( 'NONE',  ( 0.9396926207859126468, -0.3420201433256568335, 0.000000000000000000 ) ) ;
#18279 = DIRECTION ( 'NONE',  ( 1.000000000000000000, 0.000000000000000000, 0.000000000000000000 ) ) ;
#18280 = AXIS2_PLACEMENT_3D ( 'NONE', #15337, #4293, #1115 ) ;
#18281 = VECTOR ( 'NONE', #7615, 1000.000000000000000 ) ;
#18282 = ORIENTED_EDGE ( 'NONE', *, *, #2525, .F. ) ;
#18283 = CARTESIAN_POINT ( 'NONE',  ( -109.5721339228235820, 31.03941509555038181, 39.88498244535622206 ) ) ;
#18284 = VERTEX_POINT ( 'NONE', #11909 ) ;
#18285 = ORIENTED_EDGE ( 'NONE', *, *, #18418, .F. ) ;
#18286 = ADVANCED_FACE ( 'NONE', ( #10376 ), #781, .T. ) ;
#18287 = CARTESIAN_POINT ( 'NONE',  ( 47.66508197439472383, -41.06890862491489003, 293.5832628385307999 ) ) ;
#18288 = ADVANCED_FACE ( 'NONE', ( #11713 ), #10285, .T. ) ;
#18289 = ORIENTED_EDGE ( 'NONE', *, *, #535, .F. ) ;
#18290 = EDGE_LOOP ( 'NONE', ( #12620, #4388, #13532, #10678 ) ) ;
#18291 = CARTESIAN_POINT ( 'NONE',  ( 10.11498556985160846, -62.09913334491126591, 293.5832628385307999 ) ) ;
#18292 = PRESENTATION_STYLE_ASSIGNMENT (( #13982 ) ) ;
#18293 = DIRECTION ( 'NONE',  ( 0.000000000000000000, 0.000000000000000000, -1.000000000000000000 ) ) ;
#18294 = ORIENTED_EDGE ( 'NONE', *, *, #3991, .T. ) ;
#18295 = LINE ( 'NONE', #4271, #8680 ) ;
#18296 = LINE ( 'NONE', #1092, #19760 ) ;
#18297 = ORIENTED_EDGE ( 'NONE', *, *, #370, .T. ) ;
#18298 = CARTESIAN_POINT ( 'NONE',  ( -135.1060089022257102, -65.16414933467419246, 31.46482803569396935 ) ) ;
#18299 = DIRECTION ( 'NONE',  ( 1.000000000000000000, 0.000000000000000000, 0.000000000000000000 ) ) ;
#18300 = EDGE_CURVE ( 'NONE', #14181, #10780, #2623, .T. ) ;
#18301 = CARTESIAN_POINT ( 'NONE',  ( -1.379293853801755176, 78.26059000578311498, 248.9926560891072143 ) ) ;
#18302 = ORIENTED_EDGE ( 'NONE', *, *, #9905, .F. ) ;
#18303 = CYLINDRICAL_SURFACE ( 'NONE', #2214, 3.224098631618460331 ) ;
#18304 = FACE_OUTER_BOUND ( 'NONE', #16294, .T. ) ;
#18305 = FACE_OUTER_BOUND ( 'NONE', #6262, .T. ) ;
#18306 = ADVANCED_FACE ( 'NONE', ( #2519 ), #14889, .F. ) ;
#18307 = ORIENTED_EDGE ( 'NONE', *, *, #17554, .F. ) ;
#18308 = VECTOR ( 'NONE', #3783, 1000.000000000000000 ) ;
#18309 = DIRECTION ( 'NONE',  ( -0.000000000000000000, -0.000000000000000000, -1.000000000000000000 ) ) ;
#18310 = CARTESIAN_POINT ( 'NONE',  ( 78.26059000578312919, -0.8220851292427129309, 248.9926560891072143 ) ) ;
#18311 = ORIENTED_EDGE ( 'NONE', *, *, #4004, .F. ) ;
#18312 = VERTEX_POINT ( 'NONE', #17979 ) ;
#18313 = VECTOR ( 'NONE', #14937, 1000.000000000000114 ) ;
#18314 = ORIENTED_EDGE ( 'NONE', *, *, #9980, .F. ) ;
#18315 = DIRECTION ( 'NONE',  ( 0.000000000000000000, 0.000000000000000000, 1.000000000000000000 ) ) ;
#18316 = ORIENTED_EDGE ( 'NONE', *, *, #15855, .F. ) ;
#18317 = LINE ( 'NONE', #13390, #10751 ) ;
#18318 = CARTESIAN_POINT ( 'NONE',  ( 5.693982670708940041, -0.7000608949449556029, 293.5832628385307999 ) ) ;
#18319 = ORIENTED_EDGE ( 'NONE', *, *, #4627, .T. ) ;
#18320 = CARTESIAN_POINT ( 'NONE',  ( 101.4356266330684662, -128.4750511900865888, 2.021468608508339315 ) ) ;
#18321 = FACE_OUTER_BOUND ( 'NONE', #15574, .T. ) ;
#18322 = AXIS2_PLACEMENT_3D ( 'NONE', #9269, #4673, #4565 ) ;
#18323 = AXIS2_PLACEMENT_3D ( 'NONE', #15665, #3284, #15762 ) ;
#18324 = CARTESIAN_POINT ( 'NONE',  ( 52.50000000000000711, 6.293851260911244545E-13, -105.0000000000000142 ) ) ;
#18325 = FACE_OUTER_BOUND ( 'NONE', #8785, .T. ) ;
#18326 = FACE_BOUND ( 'NONE', #18881, .T. ) ;
#18327 = CARTESIAN_POINT ( 'NONE',  ( 0.5595136366802131445, -4.349754824395698272, 9.000000000000000000 ) ) ;
#18328 = CYLINDRICAL_SURFACE ( 'NONE', #2582, 7.500000000000002665 ) ;
#18329 = DIRECTION ( 'NONE',  ( -1.000000000000000000, -0.000000000000000000, -0.000000000000000000 ) ) ;
#18330 = ORIENTED_EDGE ( 'NONE', *, *, #19291, .F. ) ;
#18331 = FACE_OUTER_BOUND ( 'NONE', #3943, .T. ) ;
#18332 = DIRECTION ( 'NONE',  ( -0.000000000000000000, -0.000000000000000000, -1.000000000000000000 ) ) ;
#18333 = ORIENTED_EDGE ( 'NONE', *, *, #8414, .T. ) ;
#18334 = VECTOR ( 'NONE', #20055, 1000.000000000000114 ) ;
#18335 = ORIENTED_EDGE ( 'NONE', *, *, #3159, .T. ) ;
#18336 = SHAPE_REPRESENTATION_RELATIONSHIP ( 'NONE' , 'NONE' ,  #13949, #16290 ) ;
#18337 = ORIENTED_EDGE ( 'NONE', *, *, #1883, .T. ) ;
#18338 = FACE_BOUND ( 'NONE', #7813, .T. ) ;
#18339 = ORIENTED_EDGE ( 'NONE', *, *, #13126, .T. ) ;
#18340 = CARTESIAN_POINT ( 'NONE',  ( -36.99387960884162396, 48.17797692984176194, 283.5832628385307999 ) ) ;
#18341 = CARTESIAN_POINT ( 'NONE',  ( 133.9068821628478929, -78.54443609883627175, 3.174243263777940083 ) ) ;
#18342 = LINE ( 'NONE', #15062, #4873 ) ;
#18343 = DIRECTION ( 'NONE',  ( -0.4693298356057531429, 0.8830229359480288309, 0.000000000000000000 ) ) ;
#18344 = DIRECTION ( 'NONE',  ( -1.000000000000000000, 0.000000000000000000, 0.000000000000000000 ) ) ;
#18345 = DIRECTION ( 'NONE',  ( 0.000000000000000000, 0.000000000000000000, 1.000000000000000000 ) ) ;
#18346 = ORIENTED_EDGE ( 'NONE', *, *, #5987, .T. ) ;
#18347 = CARTESIAN_POINT ( 'NONE',  ( -60.72073886220397299, 1.629865514042312613, 293.5832628385307999 ) ) ;
#18348 = CARTESIAN_POINT ( 'NONE',  ( -135.1060089022256818, -65.16414933467422088, 10.00000000000000888 ) ) ;
#18349 = CARTESIAN_POINT ( 'NONE',  ( 125.5405970674948719, -82.09774788367153064, -9.558221728786987725 ) ) ;
#18350 = DIRECTION ( 'NONE',  ( -0.000000000000000000, -0.000000000000000000, 1.000000000000000000 ) ) ;
#18351 = DIRECTION ( 'NONE',  ( 1.000000000000000000, 0.000000000000000000, -6.977185866873308817E-15 ) ) ;
#18352 = CARTESIAN_POINT ( 'NONE',  ( -134.7188131032333729, -72.93593548660994941, 30.00000000000000355 ) ) ;
#18353 = EDGE_CURVE ( 'NONE', #17702, #19638, #14665, .T. ) ;
#18354 = ORIENTED_EDGE ( 'NONE', *, *, #258, .T. ) ;
#18355 = CARTESIAN_POINT ( 'NONE',  ( 0.000000000000000000, 0.000000000000000000, 49.99999999999999289 ) ) ;
#18356 = ORIENTED_EDGE ( 'NONE', *, *, #2145, .T. ) ;
#18357 = ORIENTED_EDGE ( 'NONE', *, *, #18646, .F. ) ;
#18358 = VERTEX_POINT ( 'NONE', #17878 ) ;
#18359 = EDGE_CURVE ( 'NONE', #2029, #14347, #1069, .T. ) ;
#18360 = ORIENTED_EDGE ( 'NONE', *, *, #15787, .T. ) ;
#18361 = EDGE_CURVE ( 'NONE', #12098, #274, #14796, .T. ) ;
#18362 = CARTESIAN_POINT ( 'NONE',  ( -139.9219061313053487, -21.70092091026256753, 23.17206116853662579 ) ) ;
#18363 = EDGE_CURVE ( 'NONE', #17037, #7508, #19411, .T. ) ;
#18364 = FACE_OUTER_BOUND ( 'NONE', #5509, .T. ) ;
#18365 = AXIS2_PLACEMENT_3D ( 'NONE', #14661, #650, #18874 ) ;
#18366 = DIRECTION ( 'NONE',  ( 0.9848077530122062440, 0.1736481776669404620, 0.000000000000000000 ) ) ;
#18367 = ORIENTED_EDGE ( 'NONE', *, *, #18534, .F. ) ;
#18368 = VECTOR ( 'NONE', #14177, 1000.000000000000114 ) ;
#18369 = CARTESIAN_POINT ( 'NONE',  ( -78.37722339831623231, 116.0043570404596522, -9.999999999999984013 ) ) ;
#18370 = CARTESIAN_POINT ( 'NONE',  ( -73.25972925305609351, 27.53920554013712874, 248.9926560891072143 ) ) ;
#18371 = ORIENTED_EDGE ( 'NONE', *, *, #7785, .T. ) ;
#18372 = FACE_OUTER_BOUND ( 'NONE', #9779, .T. ) ;
#18373 = DIRECTION ( 'NONE',  ( 0.000000000000000000, 0.000000000000000000, 1.000000000000000000 ) ) ;
#18374 = CARTESIAN_POINT ( 'NONE',  ( -133.8332678793154003, -78.98710468785296257, 2.945529613542154923 ) ) ;
#18375 = VECTOR ( 'NONE', #2758, 1000.000000000000000 ) ;
#18376 = DIRECTION ( 'NONE',  ( -0.000000000000000000, 0.000000000000000000, -1.000000000000000000 ) ) ;
#18377 = ADVANCED_FACE ( 'NONE', ( #13346 ), #974, .F. ) ;
#18378 = DIRECTION ( 'NONE',  ( -0.000000000000000000, -1.000000000000000000, -0.000000000000000000 ) ) ;
#18379 = DIRECTION ( 'NONE',  ( 0.000000000000000000, 0.000000000000000000, -1.000000000000000000 ) ) ;
#18380 = VERTEX_POINT ( 'NONE', #7317 ) ;
#18381 = VERTEX_POINT ( 'NONE', #5587 ) ;
#18382 = CYLINDRICAL_SURFACE ( 'NONE', #7359, 62.91752772691707207 ) ;
#18383 = VECTOR ( 'NONE', #11941, 1000.000000000000114 ) ;
#18384 = VECTOR ( 'NONE', #14941, 1000.000000000000227 ) ;
#18385 = VERTEX_POINT ( 'NONE', #16341 ) ;
#18386 = ORIENTED_EDGE ( 'NONE', *, *, #14501, .T. ) ;
#18387 = PLANE ( 'NONE',  #1742 ) ;
#18388 = VERTEX_POINT ( 'NONE', #13243 ) ;
#18389 = EDGE_LOOP ( 'NONE', ( #4309, #11293, #341, #67 ) ) ;
#18390 = EDGE_CURVE ( 'NONE', #3300, #19783, #5491, .T. ) ;
#18391 = AXIS2_PLACEMENT_3D ( 'NONE', #16791, #6985, #13202 ) ;
#18392 = ADVANCED_FACE ( 'NONE', ( #15087 ), #10188, .T. ) ;
#18393 = PRODUCT_RELATED_PRODUCT_CATEGORY ( 'part', '', ( #15700 ) ) ;
#18394 = CARTESIAN_POINT ( 'NONE',  ( -39.84224160888947353, -67.36461649554519227, 110.9660488491356887 ) ) ;
#18395 = DIRECTION ( 'NONE',  ( 1.000000000000000000, 0.000000000000000000, 0.000000000000000000 ) ) ;
#18396 = ORIENTED_EDGE ( 'NONE', *, *, #8861, .T. ) ;
#18397 = CARTESIAN_POINT ( 'NONE',  ( 0.8038475772933615371, 5.196152422706624030, -9.000000000000001776 ) ) ;
#18398 = CARTESIAN_POINT ( 'NONE',  ( -59.51523122377251696, 12.14914984460740754, 293.5832628385307999 ) ) ;
#18399 = ORIENTED_EDGE ( 'NONE', *, *, #1740, .F. ) ;
#18400 = CARTESIAN_POINT ( 'NONE',  ( 56.12853591711344592, -23.22718332831461652, 283.5832628385307999 ) ) ;
#18402 = AXIS2_PLACEMENT_3D ( 'NONE', #10221, #5528, #13089 ) ;
#18401 = LINE ( 'NONE', #7344, #8763 ) ;
#18403 = AXIS2_PLACEMENT_3D ( 'NONE', #6179, #30, #9442 ) ;
#18404 = CARTESIAN_POINT ( 'NONE',  ( 7.948651060879040386, -60.22029172860440127, 283.5832628385307999 ) ) ;
#18405 = EDGE_CURVE ( 'NONE', #17256, #13906, #2570, .T. ) ;
#18406 = CARTESIAN_POINT ( 'NONE',  ( 68.46530598706794990, -37.93579148621486041, 110.9660488491357455 ) ) ;
#18407 = CIRCLE ( 'NONE', #5343, 62.91752772691707207 ) ;
#18408 = DIRECTION ( 'NONE',  ( -0.9009688679024160374, -0.4338837391175646707, 0.000000000000000000 ) ) ;
#18409 = CARTESIAN_POINT ( 'NONE',  ( -81.19240997922189251, 114.0563236116805683, 24.94044186044488143 ) ) ;
#18410 = ORIENTED_EDGE ( 'NONE', *, *, #1659, .F. ) ;
#18411 = DIRECTION ( 'NONE',  ( -1.000000000000000000, 0.000000000000000000, 6.982962677686266711E-15 ) ) ;
#18412 = DIRECTION ( 'NONE',  ( 1.000000000000000000, 0.000000000000000000, 0.000000000000000000 ) ) ;
#18413 = ORIENTED_EDGE ( 'NONE', *, *, #15024, .F. ) ;
#18414 = ORIENTED_EDGE ( 'NONE', *, *, #10494, .F. ) ;
#18415 = CARTESIAN_POINT ( 'NONE',  ( 4.189777606611760026E-13, -60.00000000000000000, -105.0000000000000142 ) ) ;
#18416 = AXIS2_PLACEMENT_3D ( 'NONE', #14414, #3467, #297 ) ;
#18417 = EDGE_CURVE ( 'NONE', #2011, #18157, #13547, .T. ) ;
#18418 = EDGE_CURVE ( 'NONE', #14186, #2886, #19797, .T. ) ;
#18419 = ORIENTED_EDGE ( 'NONE', *, *, #18527, .F. ) ;
#18420 = DIRECTION ( 'NONE',  ( 0.000000000000000000, 0.000000000000000000, -1.000000000000000000 ) ) ;
#18421 = LINE ( 'NONE', #4397, #18739 ) ;
#18422 = EDGE_LOOP ( 'NONE', ( #5291, #7141, #14258, #18929 ) ) ;
#18423 = AXIS2_PLACEMENT_3D ( 'NONE', #9379, #15624, #17675 ) ;
#18424 = CARTESIAN_POINT ( 'NONE',  ( 84.61443574188869832, -123.8565353992718343, -0.1365201778679814570 ) ) ;
#18425 = FACE_BOUND ( 'NONE', #10458, .T. ) ;
#18426 = EDGE_CURVE ( 'NONE', #18461, #1479, #4249, .T. ) ;
#18427 = EDGE_CURVE ( 'NONE', #11985, #11201, #16314, .T. ) ;
#18428 = FACE_OUTER_BOUND ( 'NONE', #19126, .T. ) ;
#18429 = DIRECTION ( 'NONE',  ( -0.9396926207859046531, -0.3420201433256790380, 0.000000000000000000 ) ) ;
#18430 = FACE_OUTER_BOUND ( 'NONE', #12101, .T. ) ;
#18431 = FACE_OUTER_BOUND ( 'NONE', #19394, .T. ) ;
#18432 = CARTESIAN_POINT ( 'NONE',  ( -25.99419088092141550, 73.82206860051556419, 132.4711112102474146 ) ) ;
#18433 = CARTESIAN_POINT ( 'NONE',  ( 97.58443926496310894, -133.8443912861144725, 31.49252049683460442 ) ) ;
#18434 = ORIENTED_EDGE ( 'NONE', *, *, #2859, .T. ) ;
#18435 = DIRECTION ( 'NONE',  ( -0.03505990758545895342, -0.9993852124581886764, 0.000000000000000000 ) ) ;
#18436 = CARTESIAN_POINT ( 'NONE',  ( 40.27908801169993325, 45.46712722958823605, 293.5832628385307999 ) ) ;
#18437 = ORIENTED_EDGE ( 'NONE', *, *, #346, .T. ) ;
#18438 = VECTOR ( 'NONE', #13005, 1000.000000000000000 ) ;
#18439 = ORIENTED_EDGE ( 'NONE', *, *, #8667, .F. ) ;
#18440 = ORIENTED_EDGE ( 'NONE', *, *, #18257, .T. ) ;
#18441 = FACE_BOUND ( 'NONE', #5999, .T. ) ;
#18442 = ORIENTED_EDGE ( 'NONE', *, *, #9134, .F. ) ;
#18443 = DIRECTION ( 'NONE',  ( -0.000000000000000000, -0.000000000000000000, 1.000000000000000000 ) ) ;
#18444 = DIRECTION ( 'NONE',  ( -0.000000000000000000, -0.000000000000000000, -1.000000000000000000 ) ) ;
#18445 = CARTESIAN_POINT ( 'NONE',  ( -175.4992877478424873, -40.00000000000000000, -9.999999999999987566 ) ) ;
#18446 = VECTOR ( 'NONE', #4824, 1000.000000000000227 ) ;
#18447 = CYLINDRICAL_SURFACE ( 'NONE', #2569, 9.999999999999994671 ) ;
#18448 = ORIENTED_EDGE ( 'NONE', *, *, #16128, .F. ) ;
#18449 = DIRECTION ( 'NONE',  ( 1.000000000000000000, 0.000000000000000000, 0.000000000000000000 ) ) ;
#18450 = DIRECTION ( 'NONE',  ( -0.000000000000000000, -0.000000000000000000, 1.000000000000000000 ) ) ;
#18451 = CARTESIAN_POINT ( 'NONE',  ( 134.3287459046948698, -75.81846210760082272, 4.971753820041441507 ) ) ;
#18452 = CARTESIAN_POINT ( 'NONE',  ( -1.396592535537253342E-14, 0.000000000000000000, 39.88498244535545467 ) ) ;
#18453 = CARTESIAN_POINT ( 'NONE',  ( 76.83212392882491315, 14.94814811854985948, 132.4711112102474146 ) ) ;
#18454 = CARTESIAN_POINT ( 'NONE',  ( -128.1750136849898638, -77.98139142652895828, 40.55909899233935079 ) ) ;
#18455 = ORIENTED_EDGE ( 'NONE', *, *, #13395, .T. ) ;
#18456 = DIRECTION ( 'NONE',  ( 1.613511099790691498E-16, -1.000000000000000000, -0.000000000000000000 ) ) ;
#18457 = AXIS2_PLACEMENT_3D ( 'NONE', #3478, #511, #6754 ) ;
#18458 = ORIENTED_EDGE ( 'NONE', *, *, #17298, .T. ) ;
#18459 = AXIS2_PLACEMENT_3D ( 'NONE', #19823, #20239, #7547 ) ;
#18460 = ORIENTED_EDGE ( 'NONE', *, *, #6897, .F. ) ;
#18461 = VERTEX_POINT ( 'NONE', #8947 ) ;
#18462 = EDGE_CURVE ( 'NONE', #15722, #9575, #15606, .T. ) ;
#18463 = CARTESIAN_POINT ( 'NONE',  ( 27.93373560431201241, 14.53487841505346445, 248.9926560891072143 ) ) ;
#18464 = CARTESIAN_POINT ( 'NONE',  ( -21.51741588379869441, 55.08582882688753557, 248.9926560891072143 ) ) ;
#18465 = ORIENTED_EDGE ( 'NONE', *, *, #12968, .F. ) ;
#18467 = CARTESIAN_POINT ( 'NONE',  ( -138.4146443278754646, -17.45363688215859810, -15.43852953348798707 ) ) ;
#18466 = VECTOR ( 'NONE', #801, 1000.000000000000000 ) ;
#18468 = DIRECTION ( 'NONE',  ( 1.000000000000000000, 0.000000000000000000, 0.000000000000000000 ) ) ;
#18469 = VERTEX_POINT ( 'NONE', #18579 ) ;
#18470 = FACE_OUTER_BOUND ( 'NONE', #6621, .T. ) ;
#18471 = DIRECTION ( 'NONE',  ( -0.000000000000000000, -0.000000000000000000, 1.000000000000000000 ) ) ;
#18472 = FACE_OUTER_BOUND ( 'NONE', #14762, .T. ) ;
#18473 = CARTESIAN_POINT ( 'NONE',  ( 0.09318607064769283965, 1.767053008364804834, 8.999999999999998224 ) ) ;
#18474 = DIRECTION ( 'NONE',  ( 0.9396926207859104263, 0.3420201433256629397, -6.456589605409169071E-15 ) ) ;
#18475 = ADVANCED_FACE ( 'NONE', ( #18470 ), #15191, .F. ) ;
#18476 = CARTESIAN_POINT ( 'NONE',  ( 128.0922826834546413, -78.05640312850610485, 48.22554480681662170 ) ) ;
#18477 = CARTESIAN_POINT ( 'NONE',  ( 47.56244194535165093, 37.78198917157335757, 283.5832628385307999 ) ) ;
#18478 = AXIS2_PLACEMENT_3D ( 'NONE', #14866, #8536, #5670 ) ;
#18479 = ORIENTED_EDGE ( 'NONE', *, *, #13026, .F. ) ;
#18480 = ADVANCED_FACE ( 'NONE', ( #13859 ), #4451, .T. ) ;
#18481 = ORIENTED_EDGE ( 'NONE', *, *, #3411, .T. ) ;
#18482 = LINE ( 'NONE', #15411, #19151 ) ;
#18483 = ORIENTED_EDGE ( 'NONE', *, *, #5616, .T. ) ;
#18484 = AXIS2_PLACEMENT_3D ( 'NONE', #7243, #17801, #13462 ) ;
#18485 = ORIENTED_EDGE ( 'NONE', *, *, #13074, .F. ) ;
#18486 = CARTESIAN_POINT ( 'NONE',  ( 1.289614712049190981, -5.590028426173843101, 293.5832628385307999 ) ) ;
#18487 = ORIENTED_EDGE ( 'NONE', *, *, #14342, .T. ) ;
#18488 = EDGE_LOOP ( 'NONE', ( #19736, #18335, #10594, #12483 ) ) ;
#18489 = EDGE_CURVE ( 'NONE', #5705, #3256, #12526, .T. ) ;
#18490 = CARTESIAN_POINT ( 'NONE',  ( -7.500000000000008882, 164.0736214083062805, 60.00000000000000000 ) ) ;
#18491 =( NAMED_UNIT ( * ) PLANE_ANGLE_UNIT ( ) SI_UNIT ( $, .RADIAN. ) );
#18492 = DIRECTION ( 'NONE',  ( -0.000000000000000000, -1.000000000000000000, -0.000000000000000000 ) ) ;
#18493 = EDGE_LOOP ( 'NONE', ( #18485, #13583, #16977, #3350 ) ) ;
#18494 = DIRECTION ( 'NONE',  ( -1.734723475976805615E-16, 3.205153653169784876E-16, -1.000000000000000000 ) ) ;
#18495 = CARTESIAN_POINT ( 'NONE',  ( -7.500000000000001776, 60.00000000000000000, -105.0000000000000142 ) ) ;
#18496 = AXIS2_PLACEMENT_3D ( 'NONE', #6852, #4639, #16171 ) ;
#18497 = VERTEX_POINT ( 'NONE', #7618 ) ;
#18498 = LINE ( 'NONE', #6334, #5443 ) ;
#18499 = CARTESIAN_POINT ( 'NONE',  ( 8.833100819207578169, 58.03804081968171147, 132.4711112102474146 ) ) ;
#18500 = DIRECTION ( 'NONE',  ( -0.000000000000000000, -0.000000000000000000, 1.000000000000000000 ) ) ;
#18501 = VECTOR ( 'NONE', #13554, 1000.000000000000000 ) ;
#18502 = EDGE_CURVE ( 'NONE', #5679, #3424, #14910, .T. ) ;
#18503 = CARTESIAN_POINT ( 'NONE',  ( -71.18887634719365565, -147.8252249328922687, 49.99999999999999289 ) ) ;
#18504 = EDGE_CURVE ( 'NONE', #9562, #11829, #9049, .T. ) ;
#18505 = CARTESIAN_POINT ( 'NONE',  ( -134.4452567384424526, -75.00213249385289771, 34.30395834063391902 ) ) ;
#18506 = DIRECTION ( 'NONE',  ( 1.000000000000000000, 0.000000000000000000, -6.976128451377902853E-15 ) ) ;
#18507 = ORIENTED_EDGE ( 'NONE', *, *, #6788, .T. ) ;
#18508 = EDGE_CURVE ( 'NONE', #270, #1270, #4199, .T. ) ;
#18509 = FACE_BOUND ( 'NONE', #10837, .T. ) ;
#18510 = CARTESIAN_POINT ( 'NONE',  ( -5.281164089014709795, -2.240720816136031690, 283.5832628385307999 ) ) ;
#18511 = VERTEX_POINT ( 'NONE', #12114 ) ;
#18512 = VECTOR ( 'NONE', #13443, 999.9999999999998863 ) ;
#18513 = ORIENTED_EDGE ( 'NONE', *, *, #6243, .F. ) ;
#18514 = FACE_OUTER_BOUND ( 'NONE', #5627, .T. ) ;
#18515 = ORIENTED_EDGE ( 'NONE', *, *, #10037, .F. ) ;
#18516 = LINE ( 'NONE', #6251, #2936 ) ;
#18517 = CONICAL_SURFACE ( 'NONE', #13608, 62.91752772691707207, 0.5206510040058940358 ) ;
#18518 = ADVANCED_FACE ( 'NONE', ( #18372 ), #19998, .T. ) ;
#18519 = DIRECTION ( 'NONE',  ( 0.000000000000000000, 0.000000000000000000, 1.000000000000000000 ) ) ;
#18520 = ORIENTED_EDGE ( 'NONE', *, *, #2630, .F. ) ;
#18521 = CARTESIAN_POINT ( 'NONE',  ( 98.78819505924182920, -132.2357222602873321, 5.087113913613924510 ) ) ;
#18522 = LINE ( 'NONE', #4502, #7024 ) ;
#18523 = CARTESIAN_POINT ( 'NONE',  ( -141.6670309912509822, -18.66040293829161811, -9.999999999999985789 ) ) ;
#18524 = FACE_OUTER_BOUND ( 'NONE', #19785, .T. ) ;
#18525 = FACE_BOUND ( 'NONE', #1249, .T. ) ;
#18526 = CARTESIAN_POINT ( 'NONE',  ( 134.1130761623740568, -69.50842595698583182, 10.00000000000000178 ) ) ;
#18527 = EDGE_CURVE ( 'NONE', #1, #13430, #6000, .T. ) ;
#18528 = PLANE ( 'NONE',  #12959 ) ;
#18529 = EDGE_CURVE ( 'NONE', #13158, #6900, #6608, .T. ) ;
#18530 = LINE ( 'NONE', #18641, #14777 ) ;
#18531 = CARTESIAN_POINT ( 'NONE',  ( 86.68385341650764531, -122.4206889339569528, 43.25796838106919751 ) ) ;
#18532 = EDGE_CURVE ( 'NONE', #12459, #6317, #1796, .T. ) ;
#18533 = ORIENTED_EDGE ( 'NONE', *, *, #10321, .F. ) ;
#18534 = EDGE_CURVE ( 'NONE', #1943, #13278, #8226, .T. ) ;
#18535 = AXIS2_PLACEMENT_3D ( 'NONE', #16050, #7036, #2135 ) ;
#18536 = DIRECTION ( 'NONE',  ( -0.8479630283625698706, 0.5300553768524376430, 0.000000000000000000 ) ) ;
#18537 = CARTESIAN_POINT ( 'NONE',  ( -77.31114765718486126, 12.23146955673672842, 248.9926560891072143 ) ) ;
#18538 = ORIENTED_EDGE ( 'NONE', *, *, #7531, .T. ) ;
#18539 = ORIENTED_EDGE ( 'NONE', *, *, #8477, .F. ) ;
#18540 = EDGE_CURVE ( 'NONE', #9011, #4491, #5197, .T. ) ;
#18541 = ORIENTED_EDGE ( 'NONE', *, *, #5358, .F. ) ;
#18542 = FACE_BOUND ( 'NONE', #16846, .T. ) ;
#18543 = ORIENTED_EDGE ( 'NONE', *, *, #9253, .T. ) ;
#18544 = CARTESIAN_POINT ( 'NONE',  ( -2.647132857508373238, -114.6332882433608376, 39.88498244535547599 ) ) ;
#18545 = LINE ( 'NONE', #20177, #10246 ) ;
#18546 = LINE ( 'NONE', #9018, #4166 ) ;
#18547 = CIRCLE ( 'NONE', #19844, 7.500000000000008882 ) ;
#18548 = ADVANCED_FACE ( 'NONE', ( #18889 ), #17660, .T. ) ;
#18549 = VECTOR ( 'NONE', #13609, 1000.000000000000000 ) ;
#18550 = DIRECTION ( 'NONE',  ( -0.000000000000000000, -0.000000000000000000, -1.000000000000000000 ) ) ;
#18551 = CARTESIAN_POINT ( 'NONE',  ( -156.4179374840092862, -52.02840013024096066, 60.00000000000000000 ) ) ;
#18552 = DIRECTION ( 'NONE',  ( 0.000000000000000000, 0.000000000000000000, -1.000000000000000000 ) ) ;
#18553 = DIRECTION ( 'NONE',  ( 0.9009688679024158153, 0.4338837391175651703, 0.000000000000000000 ) ) ;
#18554 = CYLINDRICAL_SURFACE ( 'NONE', #6231, 7.500000000000020428 ) ;
#18555 = CARTESIAN_POINT ( 'NONE',  ( -133.2542153457957284, -68.87904111072103319, -0.9529167680878568580 ) ) ;
#18556 = CARTESIAN_POINT ( 'NONE',  ( 133.3512892972266854, -81.69145041114401806, 1.787651230699585758 ) ) ;
#18557 = EDGE_CURVE ( 'NONE', #9538, #9804, #9439, .T. ) ;
#18558 = CARTESIAN_POINT ( 'NONE',  ( -28.15057869795625578, -51.51682027493055216, 110.9660488491356887 ) ) ;
#18559 = FACE_OUTER_BOUND ( 'NONE', #16230, .T. ) ;
#18560 = CARTESIAN_POINT ( 'NONE',  ( -125.9179923520565865, -81.51769904231002783, 49.42145388281251428 ) ) ;
#18561 = ORIENTED_EDGE ( 'NONE', *, *, #15491, .T. ) ;
#18562 = CARTESIAN_POINT ( 'NONE',  ( 0.000000000000000000, 0.000000000000000000, 132.4711112102474146 ) ) ;
#18563 = AXIS2_PLACEMENT_3D ( 'NONE', #18784, #8024, #9566 ) ;
#18564 = ADVANCED_FACE ( 'NONE', ( #11303 ), #9469, .T. ) ;
#18565 = VECTOR ( 'NONE', #5208, 1000.000000000000000 ) ;
#18566 = VERTEX_POINT ( 'NONE', #353 ) ;
#18567 = ORIENTED_EDGE ( 'NONE', *, *, #14038, .F. ) ;
#18568 = ORIENTED_EDGE ( 'NONE', *, *, #14219, .T. ) ;
#18569 = FACE_OUTER_BOUND ( 'NONE', #8716, .T. ) ;
#18570 = DIRECTION ( 'NONE',  ( -0.8660254037844363761, -0.5000000000000039968, -0.000000000000000000 ) ) ;
#18571 = CARTESIAN_POINT ( 'NONE',  ( -109.9999999999983515, 275.0000000000000000, 85.00000000000001421 ) ) ;
#18572 = EDGE_LOOP ( 'NONE', ( #19588, #16638, #7756, #12332 ) ) ;
#18573 = VECTOR ( 'NONE', #1019, 1000.000000000000114 ) ;
#18574 = DIRECTION ( 'NONE',  ( 0.000000000000000000, 0.000000000000000000, 1.000000000000000000 ) ) ;
#18575 = FACE_OUTER_BOUND ( 'NONE', #17987, .T. ) ;
#18576 = AXIS2_PLACEMENT_3D ( 'NONE', #13116, #17657, #11495 ) ;
#18577 = VECTOR ( 'NONE', #8679, 1000.000000000000000 ) ;
#18578 = ORIENTED_EDGE ( 'NONE', *, *, #1968, .T. ) ;
#18579 = CARTESIAN_POINT ( 'NONE',  ( 55.16472960512370349, -30.25670013172234007, 132.4711112102474146 ) ) ;
#18580 = AXIS2_PLACEMENT_3D ( 'NONE', #8085, #14339, #316 ) ;
#18581 = PLANE ( 'NONE',  #3815 ) ;
#18582 = CARTESIAN_POINT ( 'NONE',  ( 175.7155416004667643, -197.3864744618499856, -6.936210497111005848E-15 ) ) ;
#18583 = CARTESIAN_POINT ( 'NONE',  ( 3.221721112346273674, 26.70531838198836283, 14.88498244535543158 ) ) ;
#18584 = FACE_OUTER_BOUND ( 'NONE', #9310, .T. ) ;
#18585 = LINE ( 'NONE', #6414, #8101 ) ;
#18586 = PLANE ( 'NONE',  #15233 ) ;
#18587 = VERTEX_POINT ( 'NONE', #12931 ) ;
#18588 = EDGE_CURVE ( 'NONE', #15182, #8563, #15310, .T. ) ;
#18589 = ORIENTED_EDGE ( 'NONE', *, *, #10789, .F. ) ;
#18590 = ORIENTED_EDGE ( 'NONE', *, *, #12515, .F. ) ;
#18591 = VECTOR ( 'NONE', #5898, 1000.000000000000000 ) ;
#18592 = CIRCLE ( 'NONE', #1952, 12.50000000000006750 ) ;
#18593 = ORIENTED_EDGE ( 'NONE', *, *, #10607, .T. ) ;
#18594 = PLANE ( 'NONE',  #8267 ) ;
#18595 = VECTOR ( 'NONE', #14698, 1000.000000000000000 ) ;
#18596 = ORIENTED_EDGE ( 'NONE', *, *, #15257, .T. ) ;
#18597 = VERTEX_POINT ( 'NONE', #462 ) ;
#18598 = PLANE ( 'NONE',  #19875 ) ;
#18599 = EDGE_CURVE ( 'NONE', #13002, #6462, #15649, .T. ) ;
#18600 = CARTESIAN_POINT ( 'NONE',  ( -5.729042578294540888, -0.2993243175132377365, 283.5832628385307999 ) ) ;
#18601 = VERTEX_POINT ( 'NONE', #5077 ) ;
#18602 = DIRECTION ( 'NONE',  ( 6.982962677686266711E-15, 0.000000000000000000, 1.000000000000000000 ) ) ;
#18603 = DIRECTION ( 'NONE',  ( 1.000000000000000000, 0.000000000000000000, 0.000000000000000000 ) ) ;
#18604 = AXIS2_PLACEMENT_3D ( 'NONE', #5645, #19751, #16498 ) ;
#18605 = VERTEX_POINT ( 'NONE', #2002 ) ;
#18606 = CARTESIAN_POINT ( 'NONE',  ( -45.48770046196285932, -37.09555676056982065, 248.9926560891072143 ) ) ;
#18607 = DIRECTION ( 'NONE',  ( -0.000000000000000000, -0.000000000000000000, 1.000000000000000000 ) ) ;
#18608 = AXIS2_PLACEMENT_3D ( 'NONE', #3536, #2005, #14475 ) ;
#18609 = VECTOR ( 'NONE', #5893, 1000.000000000000000 ) ;
#18610 = DIRECTION ( 'NONE',  ( -1.000000000000000000, -1.613511099790693471E-16, 0.000000000000000000 ) ) ;
#18611 = DIRECTION ( 'NONE',  ( 0.000000000000000000, 0.000000000000000000, 1.000000000000000000 ) ) ;
#18612 = CARTESIAN_POINT ( 'NONE',  ( -134.5748517645101856, -74.05062141148572152, 33.20438510682525646 ) ) ;
#18613 = CARTESIAN_POINT ( 'NONE',  ( -78.74873325666423796, 115.7553402848426316, 20.84531035572755897 ) ) ;
#18614 = VERTEX_POINT ( 'NONE', #11406 ) ;
#18615 = ADVANCED_FACE ( 'NONE', ( #3431 ), #14275, .T. ) ;
#18616 = ADVANCED_FACE ( 'NONE', ( #19190 ), #3633, .F. ) ;
#18617 = CARTESIAN_POINT ( 'NONE',  ( 144.1130761623740568, -69.50842595698583182, 49.99999999999999289 ) ) ;
#18618 = DIRECTION ( 'NONE',  ( 0.000000000000000000, 0.000000000000000000, 1.000000000000000000 ) ) ;
#18619 = ORIENTED_EDGE ( 'NONE', *, *, #10414, .T. ) ;
#18620 = APPLICATION_CONTEXT ( 'automotive_design' ) ;
#18621 = EDGE_LOOP ( 'NONE', ( #8690, #2218 ) ) ;
#18622 = CARTESIAN_POINT ( 'NONE',  ( 0.000000000000000000, 0.000000000000000000, 283.5832628385307999 ) ) ;
#18623 = EDGE_LOOP ( 'NONE', ( #14420, #7605, #13436, #7870 ) ) ;
#18624 = AXIS2_PLACEMENT_3D ( 'NONE', #14908, #10299, #2342 ) ;
#18625 = CIRCLE ( 'NONE', #8809, 3.224098631618459443 ) ;
#18626 = CARTESIAN_POINT ( 'NONE',  ( 0.000000000000000000, 0.000000000000000000, 293.5832628385307999 ) ) ;
#18627 = EDGE_CURVE ( 'NONE', #345, #7406, #11195, .T. ) ;
#18628 = CARTESIAN_POINT ( 'NONE',  ( -117.2142335457653672, -12.13581325405623268, 39.88498244535627180 ) ) ;
#18629 = ORIENTED_EDGE ( 'NONE', *, *, #6418, .T. ) ;
#18630 = EDGE_CURVE ( 'NONE', #18719, #10298, #15914, .T. ) ;
#18631 = CARTESIAN_POINT ( 'NONE',  ( 95.76651288690072761, -116.1232671447739051, 9.237827461556257447 ) ) ;
#18632 = DIRECTION ( 'NONE',  ( -0.000000000000000000, -0.000000000000000000, 1.000000000000000000 ) ) ;
#18633 = EDGE_CURVE ( 'NONE', #6205, #16766, #15711, .T. ) ;
#18634 = PRODUCT_DEFINITION_SHAPE ( 'NONE', 'NONE',  #20249 ) ;
#18635 = FACE_OUTER_BOUND ( 'NONE', #2124, .T. ) ;
#18636 = FACE_OUTER_BOUND ( 'NONE', #19708, .T. ) ;
#18637 = ORIENTED_EDGE ( 'NONE', *, *, #9983, .F. ) ;
#18638 = LINE ( 'NONE', #7778, #2700 ) ;
#18639 = AXIS2_PLACEMENT_3D ( 'NONE', #8416, #18031, #13500 ) ;
#18640 = DIRECTION ( 'NONE',  ( -0.000000000000000000, -0.000000000000000000, 1.000000000000000000 ) ) ;
#18641 = CARTESIAN_POINT ( 'NONE',  ( -50.41613078340781584, 30.05702882063080494, 132.4711112102474146 ) ) ;
#18642 = AXIS2_PLACEMENT_3D ( 'NONE', #7877, #3081, #9314 ) ;
#18643 = CARTESIAN_POINT ( 'NONE',  ( 92.41621553528273125, -118.1510961661374637, 47.90971605349847096 ) ) ;
#18644 = ORIENTED_EDGE ( 'NONE', *, *, #15408, .T. ) ;
#18645 = EDGE_CURVE ( 'NONE', #19334, #2821, #13033, .T. ) ;
#18646 = EDGE_CURVE ( 'NONE', #11485, #11258, #16955, .T. ) ;
#18647 = DIRECTION ( 'NONE',  ( -0.9781142164131910732, 0.2080686897406944236, 0.000000000000000000 ) ) ;
#18648 = CARTESIAN_POINT ( 'NONE',  ( 52.50000000000000711, 6.293851260911244545E-13, -100.0000000000000000 ) ) ;
#18649 = VERTEX_POINT ( 'NONE', #18048 ) ;
#18650 = EDGE_LOOP ( 'NONE', ( #3811, #18084, #9700, #17248 ) ) ;
#18651 = EDGE_LOOP ( 'NONE', ( #6843, #1009, #6157, #2817 ) ) ;
#18652 = CARTESIAN_POINT ( 'NONE',  ( -102.6608643076872767, -126.6195776799898312, 1.231354163479371433 ) ) ;
#18653 = FACE_BOUND ( 'NONE', #2296, .T. ) ;
#18654 = VERTEX_POINT ( 'NONE', #13318 ) ;
#18655 = ADVANCED_FACE ( 'NONE', ( #2601 ), #7295, .F. ) ;
#18656 = VECTOR ( 'NONE', #17710, 1000.000000000000114 ) ;
#18657 = CARTESIAN_POINT ( 'NONE',  ( 97.50000000000001421, -133.9542832461881119, 1.387778780781445676E-14 ) ) ;
#18658 = DIRECTION ( 'NONE',  ( 1.000000000000000000, 0.000000000000000000, 0.000000000000000000 ) ) ;
#18659 = CARTESIAN_POINT ( 'NONE',  ( 32.16802499836741447, 54.07248341783265033, 248.9926560891072143 ) ) ;
#18660 = ADVANCED_FACE ( 'NONE', ( #8829 ), #3727, .F. ) ;
#18661 = ADVANCED_FACE ( 'NONE', ( #1046 ), #7002, .T. ) ;
#18662 = CARTESIAN_POINT ( 'NONE',  ( -90.38423273153478021, -119.7175801288912851, 46.68965822980387514 ) ) ;
#18663 = DIRECTION ( 'NONE',  ( -0.000000000000000000, -0.000000000000000000, 1.000000000000000000 ) ) ;
#18664 = DIRECTION ( 'NONE',  ( -0.000000000000000000, -0.000000000000000000, 1.000000000000000000 ) ) ;
#18665 = DIRECTION ( 'NONE',  ( 0.000000000000000000, 0.000000000000000000, 1.000000000000000000 ) ) ;
#18666 = FACE_OUTER_BOUND ( 'NONE', #6773, .T. ) ;
#18667 = CARTESIAN_POINT ( 'NONE',  ( 131.5402663983728360, -89.84204999195762298, 0.05619734976503784618 ) ) ;
#18668 = CARTESIAN_POINT ( 'NONE',  ( -24.73834469112697576, -10.56256686379325593, 14.88498244535562520 ) ) ;
#18669 = DIRECTION ( 'NONE',  ( -0.000000000000000000, -0.000000000000000000, 1.000000000000000000 ) ) ;
#18670 = CARTESIAN_POINT ( 'NONE',  ( -133.9275976130222432, -67.55320356804372750, 38.83589090172372238 ) ) ;
#18671 = ORIENTED_EDGE ( 'NONE', *, *, #14144, .T. ) ;
#18672 = CIRCLE ( 'NONE', #11774, 10.00000000000000533 ) ;
#18673 = EDGE_CURVE ( 'NONE', #7733, #1943, #16418, .T. ) ;
#18674 = CARTESIAN_POINT ( 'NONE',  ( -0.8220851292435327196, -78.26059000578311498, 112.7772637782949943 ) ) ;
#18675 = CIRCLE ( 'NONE', #3639, 7.500000000000007105 ) ;
#18676 = ORIENTED_EDGE ( 'NONE', *, *, #6758, .T. ) ;
#18677 = ORIENTED_EDGE ( 'NONE', *, *, #7772, .T. ) ;
#18678 = AXIS2_PLACEMENT_3D ( 'NONE', #12814, #8212, #14457 ) ;
#18679 = ORIENTED_EDGE ( 'NONE', *, *, #1990, .F. ) ;
#18680 = EDGE_CURVE ( 'NONE', #4551, #5660, #5566, .T. ) ;
#18681 = EDGE_CURVE ( 'NONE', #12139, #9304, #11498, .T. ) ;
#18682 = CARTESIAN_POINT ( 'NONE',  ( 4.811834253409010387, 3.123743752084098269, 293.5832628385307999 ) ) ;
#18683 = CARTESIAN_POINT ( 'NONE',  ( 0.000000000000000000, 0.000000000000000000, 283.5832628385307999 ) ) ;
#18684 = VERTEX_POINT ( 'NONE', #14676 ) ;
#18685 = CARTESIAN_POINT ( 'NONE',  ( 60.22029172860436574, 7.948651060879242003, 283.5832628385307999 ) ) ;
#18686 = CARTESIAN_POINT ( 'NONE',  ( 45.46865632508072963, -40.28046525994365368, 293.5832628385307999 ) ) ;
#18687 = EDGE_CURVE ( 'NONE', #1807, #19254, #14678, .T. ) ;
#18688 = CARTESIAN_POINT ( 'NONE',  ( -105.2523856663880366, 80.72709874070729086, -29.68324780735369472 ) ) ;
#18689 = CARTESIAN_POINT ( 'NONE',  ( 59.51523122377253117, -12.14914984460739156, 283.5832628385307999 ) ) ;
#18690 = CARTESIAN_POINT ( 'NONE',  ( 178.1870518357301023, -192.0755223619200081, 4.142135623730942129 ) ) ;
#18691 = DIRECTION ( 'NONE',  ( 6.982962677686266711E-15, -0.000000000000000000, 1.000000000000000000 ) ) ;
#18692 = CARTESIAN_POINT ( 'NONE',  ( -20.84572577951200500, -54.86954475316249358, 111.4180192758973931 ) ) ;
#18693 = CARTESIAN_POINT ( 'NONE',  ( -23.19741967113651882, 4.658826548058537576, 39.88498244535561810 ) ) ;
#18694 = CARTESIAN_POINT ( 'NONE',  ( 71.18887634719571622, -147.8252249328912740, 60.00000000000000000 ) ) ;
#18695 = ORIENTED_EDGE ( 'NONE', *, *, #2665, .T. ) ;
#18696 = VERTEX_POINT ( 'NONE', #17753 ) ;
#18697 = EDGE_LOOP ( 'NONE', ( #4783, #17290, #17720, #5450 ) ) ;
#18698 = VERTEX_POINT ( 'NONE', #11786 ) ;
#18699 = DIRECTION ( 'NONE',  ( -1.000000000000000000, 0.000000000000000000, 0.000000000000000000 ) ) ;
#18700 = AXIS2_PLACEMENT_3D ( 'NONE', #17639, #39, #14049 ) ;
#18701 = EDGE_LOOP ( 'NONE', ( #18116, #13301 ) ) ;
#18702 = DIRECTION ( 'NONE',  ( 0.9396926207859092051, -0.3420201433256662704, -0.000000000000000000 ) ) ;
#18703 = PLANE ( 'NONE',  #11060 ) ;
#18704 = CARTESIAN_POINT ( 'NONE',  ( -50.13752642112849855, -30.53958573130890741, 110.9660488491356887 ) ) ;
#18705 = CARTESIAN_POINT ( 'NONE',  ( 135.7779226595531270, 102.2982297021113141, 39.99999999999999289 ) ) ;
#18706 = ORIENTED_EDGE ( 'NONE', *, *, #12400, .F. ) ;
#18707 = CARTESIAN_POINT ( 'NONE',  ( 85.53020504959901871, -140.9188050298377846, 60.00000000000000000 ) ) ;
#18708 = DIRECTION ( 'NONE',  ( 0.000000000000000000, 0.000000000000000000, 1.000000000000000000 ) ) ;
#18709 = ORIENTED_EDGE ( 'NONE', *, *, #8475, .F. ) ;
#18710 = UNCERTAINTY_MEASURE_WITH_UNIT (LENGTH_MEASURE( 1.000000000000000082E-05 ), #14131, 'distance_accuracy_value', 'NONE');
#18711 = CARTESIAN_POINT ( 'NONE',  ( -73.97516692619829826, 130.4256996493784015, -12.43080227311476449 ) ) ;
#18712 = CARTESIAN_POINT ( 'NONE',  ( -86.01343624116279329, 31.38211805825948630, 30.00000000000000000 ) ) ;
#18713 = DIRECTION ( 'NONE',  ( -1.613511099790691498E-16, 1.000000000000000000, 0.000000000000000000 ) ) ;
#18714 = AXIS2_PLACEMENT_3D ( 'NONE', #10668, #3215, #9458 ) ;
#18715 = VECTOR ( 'NONE', #12790, 1000.000000000000000 ) ;
#18716 = DIRECTION ( 'NONE',  ( 6.982962677686266711E-15, -0.000000000000000000, 1.000000000000000000 ) ) ;
#18717 = DIRECTION ( 'NONE',  ( 0.000000000000000000, 0.000000000000000000, -1.000000000000000000 ) ) ;
#18718 = CARTESIAN_POINT ( 'NONE',  ( -90.12511548116496840, 107.1354966152653390, 33.81810546212673785 ) ) ;
#18719 = VERTEX_POINT ( 'NONE', #5465 ) ;
#18720 = CARTESIAN_POINT ( 'NONE',  ( 0.000000000000000000, 0.000000000000000000, 293.5832628385307999 ) ) ;
#18721 = VERTEX_POINT ( 'NONE', #14963 ) ;
#18722 = CIRCLE ( 'NONE', #732, 106.4288957539801288 ) ;
#18723 = ORIENTED_EDGE ( 'NONE', *, *, #18687, .T. ) ;
#18724 = CARTESIAN_POINT ( 'NONE',  ( 75.91068486117727332, -120.9436655338208340, 39.99999999999999289 ) ) ;
#18725 = EDGE_LOOP ( 'NONE', ( #15447, #6873, #1037, #3893 ) ) ;
#18726 = CARTESIAN_POINT ( 'NONE',  ( -71.18887634719365565, -147.8252249328922687, 49.99999999999999289 ) ) ;
#18727 = CARTESIAN_POINT ( 'NONE',  ( 6.445787855800395547E-13, 1.379293853801755176, 248.9926560891072143 ) ) ;
#18728 = AXIS2_PLACEMENT_3D ( 'NONE', #10339, #5752, #18128 ) ;
#18729 = ORIENTED_EDGE ( 'NONE', *, *, #10587, .T. ) ;
#18730 = AXIS2_PLACEMENT_3D ( 'NONE', #808, #16275, #19143 ) ;
#18731 = CARTESIAN_POINT ( 'NONE',  ( 97.47038759843226785, -115.4903015188358495, 10.15380083008228596 ) ) ;
#18732 = CARTESIAN_POINT ( 'NONE',  ( -12.78021302872797449, 77.21438937758516374, 132.4711112102474146 ) ) ;
#18733 = ADVANCED_FACE ( 'NONE', ( #10353 ), #16614, .T. ) ;
#18734 = VECTOR ( 'NONE', #1185, 1000.000000000000000 ) ;
#18735 = CARTESIAN_POINT ( 'NONE',  ( -77.50000000000000000, 9.491012693391988181E-15, -115.0000000000000000 ) ) ;
#18736 = CARTESIAN_POINT ( 'NONE',  ( -48.72193424476478896, -39.80940113486003185, 132.4711112102474146 ) ) ;
#18737 = ORIENTED_EDGE ( 'NONE', *, *, #1272, .T. ) ;
#18738 = DIRECTION ( 'NONE',  ( -0.000000000000000000, -0.000000000000000000, -1.000000000000000000 ) ) ;
#18739 = VECTOR ( 'NONE', #10623, 1000.000000000000000 ) ;
#18740 = PLANE ( 'NONE',  #561 ) ;
#18741 = DIRECTION ( 'NONE',  ( -0.000000000000000000, -0.000000000000000000, 1.000000000000000000 ) ) ;
#18742 = CARTESIAN_POINT ( 'NONE',  ( 102.7654166546833210, -126.4532151214411186, 38.81363406805538574 ) ) ;
#18743 = VERTEX_POINT ( 'NONE', #9968 ) ;
#18744 = ADVANCED_FACE ( 'NONE', ( #10069 ), #10166, .T. ) ;
#18745 = CARTESIAN_POINT ( 'NONE',  ( -79.05640494597939494, -127.4758205975444412, 49.99999999999999289 ) ) ;
#18746 = CARTESIAN_POINT ( 'NONE',  ( 0.000000000000000000, 164.0736214083062805, 49.99999999999999289 ) ) ;
#18747 = ADVANCED_FACE ( 'NONE', ( #5273 ), #952, .T. ) ;
#18748 = ORIENTED_EDGE ( 'NONE', *, *, #19162, .T. ) ;
#18749 = ORIENTED_EDGE ( 'NONE', *, *, #4802, .F. ) ;
#18750 = ADVANCED_FACE ( 'NONE', ( #10260 ), #16517, .F. ) ;
#18751 = ORIENTED_EDGE ( 'NONE', *, *, #15121, .T. ) ;
#18752 = CARTESIAN_POINT ( 'NONE',  ( -30.00000000000001421, 292.9500000000000455, 4.999999999999130473 ) ) ;
#18753 = CIRCLE ( 'NONE', #5357, 62.91752772691707207 ) ;
#18754 = EDGE_LOOP ( 'NONE', ( #14832, #9277, #4024, #5618 ) ) ;
#18755 = CARTESIAN_POINT ( 'NONE',  ( 0.000000000000000000, 0.000000000000000000, 248.9926560891072143 ) ) ;
#18756 = FACE_BOUND ( 'NONE', #7090, .T. ) ;
#18757 = AXIS2_PLACEMENT_3D ( 'NONE', #5122, #14422, #19132 ) ;
#18758 = VERTEX_POINT ( 'NONE', #16321 ) ;
#18759 = CYLINDRICAL_SURFACE ( 'NONE', #18403, 7.500000000000007105 ) ;
#18760 = CARTESIAN_POINT ( 'NONE',  ( -74.01264520835138683, 25.47058595421627913, 248.9926560891072143 ) ) ;
#18761 = CARTESIAN_POINT ( 'NONE',  ( -82.03125000082627594, -125.5821405427617066, 8.489866645478734597 ) ) ;
#18762 = ADVANCED_FACE ( 'NONE', ( #19673 ), #18143, .F. ) ;
#18763 = CARTESIAN_POINT ( 'NONE',  ( -84.12762954502584023, -124.1876770196617343, 39.19636848888279701 ) ) ;
#18764 = DIRECTION ( 'NONE',  ( -1.613511099790691498E-16, 1.000000000000000000, -0.000000000000000000 ) ) ;
#18765 = CARTESIAN_POINT ( 'NONE',  ( -139.1630865236926695, 15.78015590158507031, 24.36223180621681195 ) ) ;
#18766 = LINE ( 'NONE', #1984, #16089 ) ;
#18767 = AXIS2_PLACEMENT_3D ( 'NONE', #9949, #9743, #14656 ) ;
#18768 = DIRECTION ( 'NONE',  ( 0.000000000000000000, -1.000000000000000000, -3.338476886082585705E-16 ) ) ;
#18769 = CARTESIAN_POINT ( 'NONE',  ( -79.05640494597940915, -127.4758205975444270, 60.00000000000000000 ) ) ;
#18770 = CARTESIAN_POINT ( 'NONE',  ( -124.7133609680327311, -83.36099555805665773, 40.87838703930916751 ) ) ;
#18771 = ORIENTED_EDGE ( 'NONE', *, *, #11268, .T. ) ;
#18772 = EDGE_CURVE ( 'NONE', #8175, #4586, #2305, .T. ) ;
#18773 = CARTESIAN_POINT ( 'NONE',  ( 22.81000261549368346, -58.63718168490493099, 293.5832628385307999 ) ) ;
#18774 = VECTOR ( 'NONE', #17352, 1000.000000000000000 ) ;
#18775 = ADVANCED_FACE ( 'NONE', ( #10768 ), #16711, .F. ) ;
#18776 = EDGE_CURVE ( 'NONE', #3219, #14755, #2696, .T. ) ;
#18777 = EDGE_LOOP ( 'NONE', ( #6299, #2912, #3172, #10077 ) ) ;
#18778 = ORIENTED_EDGE ( 'NONE', *, *, #18004, .T. ) ;
#18779 = ORIENTED_EDGE ( 'NONE', *, *, #6786, .T. ) ;
#18780 = AXIS2_PLACEMENT_3D ( 'NONE', #19338, #5323, #5719 ) ;
#18781 = CARTESIAN_POINT ( 'NONE',  ( -142.1121543937410081, -17.96810325432989686, 18.92822252394145011 ) ) ;
#18782 = ADVANCED_FACE ( 'NONE', ( #3110 ), #16812, .F. ) ;
#18783 = PLANE ( 'NONE',  #19104 ) ;
#18784 = CARTESIAN_POINT ( 'NONE',  ( 159.9599531637113330, -36.50981547336952104, 49.99999999999999289 ) ) ;
#18785 = DIRECTION ( 'NONE',  ( 6.982962677686266711E-15, 0.000000000000000000, 1.000000000000000000 ) ) ;
#18786 = CARTESIAN_POINT ( 'NONE',  ( -0.2993243175131981570, 5.729042578294444077, 293.5832628385307999 ) ) ;
#18787 = CYLINDRICAL_SURFACE ( 'NONE', #12806, 112.8770930172170210 ) ;
#18788 = CARTESIAN_POINT ( 'NONE',  ( -167.4599531637108782, -36.50981547337168109, 39.99999999999999289 ) ) ;
#18789 = FACE_OUTER_BOUND ( 'NONE', #2346, .T. ) ;
#18790 = VECTOR ( 'NONE', #16041, 1000.000000000000000 ) ;
#18791 = DIRECTION ( 'NONE',  ( 0.9848077530122062440, 0.1736481776669404620, 0.000000000000000000 ) ) ;
#18792 = EDGE_LOOP ( 'NONE', ( #8318, #15956, #5236 ) ) ;
#18793 = EDGE_CURVE ( 'NONE', #14390, #10728, #14015, .T. ) ;
#18794 = CARTESIAN_POINT ( 'NONE',  ( 131.5110516633172040, -72.14693729182981485, 44.44710436446363389 ) ) ;
#18795 = AXIS2_PLACEMENT_3D ( 'NONE', #3881, #5617, #18098 ) ;
#18796 = DIRECTION ( 'NONE',  ( -0.9781142164131917394, 0.2080686897406911207, 0.000000000000000000 ) ) ;
#18797 = ADVANCED_FACE ( 'NONE', ( #12298 ), #15169, .F. ) ;
#18798 = EDGE_LOOP ( 'NONE', ( #19839, #2530, #5884, #16229 ) ) ;
#18799 = ORIENTED_EDGE ( 'NONE', *, *, #17902, .T. ) ;
#18800 = ORIENTED_EDGE ( 'NONE', *, *, #3855, .T. ) ;
#18801 = EDGE_CURVE ( 'NONE', #12677, #10504, #1363, .T. ) ;
#18802 = ORIENTED_EDGE ( 'NONE', *, *, #16160, .T. ) ;
#18803 = DIRECTION ( 'NONE',  ( 0.5000000000000069944, -0.8660254037844344888, 0.000000000000000000 ) ) ;
#18804 = PRODUCT ( 'hex bolt gradec_iso_ISO 4016 - M12 x 55 x 30-WN', 'hex bolt gradec_iso_ISO 4016 - M12 x 55 x 30-WN', '', ( #20170 ) ) ;
#18805 = ORIENTED_EDGE ( 'NONE', *, *, #5628, .F. ) ;
#18806 = CARTESIAN_POINT ( 'NONE',  ( 0.000000000000000000, 0.000000000000000000, 0.000000000000000000 ) ) ;
#18807 = VECTOR ( 'NONE', #1196, 1000.000000000000000 ) ;
#18808 = FACE_OUTER_BOUND ( 'NONE', #16881, .T. ) ;
#18809 = DIRECTION ( 'NONE',  ( 6.982962677686266711E-15, 0.000000000000000000, 1.000000000000000000 ) ) ;
#18810 =( LENGTH_UNIT ( ) NAMED_UNIT ( * ) SI_UNIT ( .MILLI., .METRE. ) );
#18811 = EDGE_CURVE ( 'NONE', #4702, #14163, #17983, .T. ) ;
#18812 = CARTESIAN_POINT ( 'NONE',  ( 7.948937137877743808, -60.22232964560488000, 283.5832628385307999 ) ) ;
#18813 = ORIENTED_EDGE ( 'NONE', *, *, #9760, .F. ) ;
#18814 = CARTESIAN_POINT ( 'NONE',  ( 122.8001410695374602, -86.14014948502067170, -10.00000000000000178 ) ) ;
#18815 = CARTESIAN_POINT ( 'NONE',  ( -28.43859219408707872, 46.49849886828685896, 248.9926560891072143 ) ) ;
#18816 = EDGE_LOOP ( 'NONE', ( #4527, #18619, #7485, #6863 ) ) ;
#18817 =( BOUNDED_SURFACE ( )  B_SPLINE_SURFACE ( 3, 2, ( 
 ( #5775, #5879, #18352 ),
 ( #10360, #1052, #12201 ),
 ( #5980, #11793, #15174 ),
 ( #15072, #16522, #4329 ),
 ( #2502, #11890, #11991 ),
 ( #16817, #13737, #3664 ),
 ( #9898, #13325, #19581 ),
 ( #17234, #12410, #1369 ),
 ( #18872, #13841, #2910 ),
 ( #18670, #10666, #6493 ),
 ( #15698, #13944, #1471 ),
 ( #17129, #20189, #6192 ),
 ( #7702, #14053, #9138 ),
 ( #10873, #1780, #14257 ),
 ( #7599, #15379, #3318 ),
 ( #20084, #10975, #8011 ),
 ( #9554, #1576, #42 ),
 ( #15799, #4647, #6392 ),
 ( #17342, #3115, #16921 ),
 ( #4752, #6293, #240 ),
 ( #6084, #18454, #9345 ),
 ( #15592, #1680, #7811 ),
 ( #12507, #11078, #4437 ),
 ( #12302, #15487, #3213 ),
 ( #9454, #4542, #3012 ),
 ( #18560, #17026, #9244 ),
 ( #10773, #18770, #7907 ),
 ( #14154, #140, #12610 ),
 ( #4857, #14659, #16203 ),
 ( #1878, #2190, #16099 ) ),
 .UNSPECIFIED., .F., .F., .F. ) 
 B_SPLINE_SURFACE_WITH_KNOTS ( ( 4, 2, 2, 2, 2, 2, 2, 2, 2, 2, 2, 2, 2, 2, 4 ),
 ( 3, 3 ),
 ( 0.01087485647533277880, 0.01538493460406631895, 0.01651245413624970529, 0.01763997366843308989, 0.01989501273279985910, 0.02102253226498324370, 0.02215005179716662831, 0.02440509086153340099, 0.02891516899026694287, 0.03117020805463371208, 0.03342524711900048129, 0.03793532524773401970, 0.04019036431210078891, 0.04244540337646755812, 0.04695548150520110348 ),
 ( 0.000000000000000000, 1.000000000000000000 ),
 .UNSPECIFIED. ) 
 GEOMETRIC_REPRESENTATION_ITEM ( )  RATIONAL_B_SPLINE_SURFACE ( (
 ( 1.000000000000000000, 0.9212076576725557464, 1.000000000000000000),
 ( 1.000000000000000000, 0.9211983545445763255, 1.000000000000000000),
 ( 1.000000000000000000, 0.9192884530626878048, 1.000000000000000000),
 ( 1.000000000000000000, 0.9147257148664106330, 1.000000000000000000),
 ( 1.000000000000000000, 0.9137002753874979843, 1.000000000000000000),
 ( 1.000000000000000000, 0.9114460110780681079, 1.000000000000000000),
 ( 1.000000000000000000, 0.9102239901659594512, 1.000000000000000000),
 ( 1.000000000000000000, 0.9062907615861804933, 1.000000000000000000),
 ( 1.000000000000000000, 0.9033134084428574573, 1.000000000000000000),
 ( 1.000000000000000000, 0.8983619464026600943, 1.000000000000000000),
 ( 1.000000000000000000, 0.8966302762932344406, 1.000000000000000000),
 ( 1.000000000000000000, 0.8930095736512829729, 1.000000000000000000),
 ( 1.000000000000000000, 0.8911146393079628636, 1.000000000000000000),
 ( 1.000000000000000000, 0.8852539528816872894, 1.000000000000000000),
 ( 1.000000000000000000, 0.8811119717501607607, 1.000000000000000000),
 ( 1.000000000000000000, 0.8680569459629184914, 1.000000000000000000),
 ( 1.000000000000000000, 0.8585210289499386471, 1.000000000000000000),
 ( 1.000000000000000000, 0.8431029601255346506, 1.000000000000000000),
 ( 1.000000000000000000, 0.8377859708359541857, 1.000000000000000000),
 ( 1.000000000000000000, 0.8269824639699362434, 1.000000000000000000),
 ( 1.000000000000000000, 0.8214732595401645909, 1.000000000000000000),
 ( 1.000000000000000000, 0.8046428831057845787, 1.000000000000000000),
 ( 1.000000000000000000, 0.7930208592507520526, 1.000000000000000000),
 ( 1.000000000000000000, 0.7750195416465174292, 1.000000000000000000),
 ( 1.000000000000000000, 0.7688986879966103194, 1.000000000000000000),
 ( 1.000000000000000000, 0.7566232400044657913, 1.000000000000000000),
 ( 1.000000000000000000, 0.7504663834238096687, 1.000000000000000000),
 ( 1.000000000000000000, 0.7319497228662610322, 1.000000000000000000),
 ( 1.000000000000000000, 0.7195437534939763680, 1.000000000000000000),
 ( 1.000000000000000000, 0.7071067811865474617, 1.000000000000000000) ) ) 
 REPRESENTATION_ITEM ( '' )  SURFACE ( )  );
#18818 = DIRECTION ( 'NONE',  ( 1.000000000000000000, 0.000000000000000000, 0.000000000000000000 ) ) ;
#18819 = DIRECTION ( 'NONE',  ( 1.000000000000000000, 0.000000000000000000, -0.000000000000000000 ) ) ;
#18820 = VECTOR ( 'NONE', #15097, 1000.000000000000000 ) ;
#18821 = DIRECTION ( 'NONE',  ( 0.000000000000000000, 0.000000000000000000, 1.000000000000000000 ) ) ;
#18822 = CARTESIAN_POINT ( 'NONE',  ( 8.938941455415006843, -60.08127757648380651, 283.5832628385307999 ) ) ;
#18823 = CARTESIAN_POINT ( 'NONE',  ( 60.72073886220397299, -1.629865514042299734, 283.5832628385307999 ) ) ;
#18824 = CARTESIAN_POINT ( 'NONE',  ( 85.33507189799762216, -123.3618359587737672, 41.35839226945913794 ) ) ;
#18825 = ORIENTED_EDGE ( 'NONE', *, *, #4389, .F. ) ;
#18826 = CYLINDRICAL_SURFACE ( 'NONE', #14485, 7.500000000000020428 ) ;
#18827 = ORIENTED_EDGE ( 'NONE', *, *, #12108, .T. ) ;
#18828 = EDGE_CURVE ( 'NONE', #19621, #14853, #13731, .T. ) ;
#18829 = VERTEX_POINT ( 'NONE', #16916 ) ;
#18830 = CARTESIAN_POINT ( 'NONE',  ( 0.000000000000000000, 0.000000000000000000, -9.999999999999994671 ) ) ;
#18831 = ORIENTED_EDGE ( 'NONE', *, *, #10357, .T. ) ;
#18832 = VECTOR ( 'NONE', #607, 1000.000000000000000 ) ;
#18833 = CARTESIAN_POINT ( 'NONE',  ( -133.9520938386737043, 58.56720361986037915, -27.05300300615894571 ) ) ;
#18834 = CARTESIAN_POINT ( 'NONE',  ( -71.18887634719365565, -147.8252249328922687, 39.99999999999999289 ) ) ;
#18835 = ORIENTED_EDGE ( 'NONE', *, *, #16443, .T. ) ;
#18836 = CARTESIAN_POINT ( 'NONE',  ( 99.15486248080401310, -131.7338018236151527, 4.478766899919759403 ) ) ;
#18837 = LINE ( 'NONE', #18732, #1800 ) ;
#18838 = VECTOR ( 'NONE', #201, 1000.000000000000000 ) ;
#18839 = CARTESIAN_POINT ( 'NONE',  ( 51.77251465595239921, -31.77296517111717478, 293.5832628385307999 ) ) ;
#18840 = CARTESIAN_POINT ( 'NONE',  ( -54.67896814532655725, -21.36933070621745046, 132.4711112102474146 ) ) ;
#18841 = ORIENTED_EDGE ( 'NONE', *, *, #7746, .F. ) ;
#18842 = CYLINDRICAL_SURFACE ( 'NONE', #11516, 32.50000000000000000 ) ;
#18843 = CARTESIAN_POINT ( 'NONE',  ( 0.000000000000000000, 0.000000000000000000, 283.5832628385307999 ) ) ;
#18844 = CARTESIAN_POINT ( 'NONE',  ( -50.37374754117254838, -141.2886604036510505, 49.99999999999999289 ) ) ;
#18845 = CARTESIAN_POINT ( 'NONE',  ( 96.93610878393036501, -115.7104363121800077, 29.64800143911388020 ) ) ;
#18846 = ORIENTED_EDGE ( 'NONE', *, *, #15723, .F. ) ;
#18847 = CARTESIAN_POINT ( 'NONE',  ( -7.948651060879021735, 60.22029172860445101, 283.5832628385307999 ) ) ;
#18848 = CARTESIAN_POINT ( 'NONE',  ( -77.10567499969560856, 128.6696624883277309, 27.82549893712029387 ) ) ;
#18849 = VERTEX_POINT ( 'NONE', #19872 ) ;
#18850 = EDGE_CURVE ( 'NONE', #7238, #4761, #6883, .T. ) ;
#18851 = ORIENTED_EDGE ( 'NONE', *, *, #18919, .F. ) ;
#18853 = ORIENTED_EDGE ( 'NONE', *, *, #9894, .F. ) ;
#18852 = CIRCLE ( 'NONE', #19176, 3.224098631618461219 ) ;
#18854 = VERTEX_POINT ( 'NONE', #18347 ) ;
#18855 = CARTESIAN_POINT ( 'NONE',  ( -104.1536737562094288, -124.2508859553632306, 0.5727794066519206195 ) ) ;
#18856 = DIRECTION ( 'NONE',  ( 0.9396926207859069846, 0.3420201433256726542, 0.000000000000000000 ) ) ;
#18857 = ORIENTED_EDGE ( 'NONE', *, *, #14116, .F. ) ;
#18858 = DIRECTION ( 'NONE',  ( 1.000000000000000000, 0.000000000000000000, 0.000000000000000000 ) ) ;
#18859 = CARTESIAN_POINT ( 'NONE',  ( 8.939227532413712041, -60.08331549348429235, 283.5832628385307999 ) ) ;
#18860 = CARTESIAN_POINT ( 'NONE',  ( 126.0064496073183307, -81.39031533630308957, 49.41728923137324614 ) ) ;
#18861 = AXIS2_PLACEMENT_3D ( 'NONE', #5103, #11433, #11331 ) ;
#18862 = VECTOR ( 'NONE', #8405, 1000.000000000000000 ) ;
#18863 = EDGE_CURVE ( 'NONE', #1487, #17498, #9340, .T. ) ;
#18864 = CARTESIAN_POINT ( 'NONE',  ( -99.76899065921458032, -130.8788316638204492, 36.35208880440197277 ) ) ;
#18865 = CARTESIAN_POINT ( 'NONE',  ( 0.000000000000000000, 0.000000000000000000, 49.99999999999999289 ) ) ;
#18866 = CARTESIAN_POINT ( 'NONE',  ( -140.0000000000000568, 2.005623917688350133, 23.02775637731988212 ) ) ;
#18867 = DIRECTION ( 'NONE',  ( 0.7660444431189858960, -0.6427876096865300370, 0.000000000000000000 ) ) ;
#18868 = AXIS2_PLACEMENT_3D ( 'NONE', #8287, #15972, #13 ) ;
#18869 = DIRECTION ( 'NONE',  ( 0.000000000000000000, 1.000000000000000000, 0.000000000000000000 ) ) ;
#18870 = FACE_OUTER_BOUND ( 'NONE', #6275, .T. ) ;
#18871 = CARTESIAN_POINT ( 'NONE',  ( 0.000000000000000000, 0.000000000000000000, 283.5832628385307999 ) ) ;
#18872 = CARTESIAN_POINT ( 'NONE',  ( -134.1858200530606950, -67.03963421359212305, 37.88757044792966866 ) ) ;
#18873 = ORIENTED_EDGE ( 'NONE', *, *, #11954, .T. ) ;
#18874 = DIRECTION ( 'NONE',  ( -0.1736481776669268895, 0.9848077530122086864, 1.076098267568195240E-15 ) ) ;
#18875 = ADVANCED_FACE ( 'NONE', ( #19976 ), #15586, .F. ) ;
#18876 = ORIENTED_EDGE ( 'NONE', *, *, #19857, .F. ) ;
#18877 = VECTOR ( 'NONE', #18492, 1000.000000000000000 ) ;
#18878 = ORIENTED_EDGE ( 'NONE', *, *, #8373, .F. ) ;
#18879 = AXIS2_PLACEMENT_3D ( 'NONE', #16668, #2656, #16971 ) ;
#18880 = AXIS2_PLACEMENT_3D ( 'NONE', #10994, #3233, #1697 ) ;
#18881 = EDGE_LOOP ( 'NONE', ( #14980, #19960 ) ) ;
#18882 = CARTESIAN_POINT ( 'NONE',  ( -143.8108380990476576, -15.58935400314438446, -4.058802881218986691 ) ) ;
#18883 = CARTESIAN_POINT ( 'NONE',  ( 0.000000000000000000, 0.000000000000000000, 293.5832628385307999 ) ) ;
#18884 = EDGE_CURVE ( 'NONE', #269, #11053, #19601, .T. ) ;
#18885 = CYLINDRICAL_SURFACE ( 'NONE', #4848, 62.91752772691707207 ) ;
#18886 = CARTESIAN_POINT ( 'NONE',  ( 0.000000000000000000, 0.000000000000000000, -120.0000000000000142 ) ) ;
#18887 = ORIENTED_EDGE ( 'NONE', *, *, #6004, .T. ) ;
#18888 = EDGE_CURVE ( 'NONE', #1786, #14795, #10445, .T. ) ;
#18889 = FACE_OUTER_BOUND ( 'NONE', #7729, .T. ) ;
#18890 = FACE_OUTER_BOUND ( 'NONE', #14594, .T. ) ;
#18891 = CARTESIAN_POINT ( 'NONE',  ( 71.18887634719571622, -147.8252249328912740, 49.99999999999999289 ) ) ;
#18892 = DIRECTION ( 'NONE',  ( -6.982962677686266711E-15, 0.000000000000000000, -1.000000000000000000 ) ) ;
#18893 = DIRECTION ( 'NONE',  ( 1.000000000000000000, 0.000000000000000000, 0.000000000000000000 ) ) ;
#18894 = CONICAL_SURFACE ( 'NONE', #12670, 62.91752772691707207, 0.5206510040058940358 ) ;
#18895 = EDGE_LOOP ( 'NONE', ( #4385, #1159, #14333, #4311 ) ) ;
#18896 = AXIS2_PLACEMENT_3D ( 'NONE', #12175, #7375, #18435 ) ;
#18897 = CARTESIAN_POINT ( 'NONE',  ( 133.2712073792189074, -68.96827650324327408, 30.52894171284383873 ) ) ;
#18898 = CARTESIAN_POINT ( 'NONE',  ( 0.000000000000000000, 0.000000000000000000, 248.9926560891072143 ) ) ;
#18899 = VERTEX_POINT ( 'NONE', #20079 ) ;
#18900 = ORIENTED_EDGE ( 'NONE', *, *, #16412, .F. ) ;
#18901 = ADVANCED_FACE ( 'NONE', ( #6078 ), #18554, .F. ) ;
#18902 = VERTEX_POINT ( 'NONE', #20184 ) ;
#18903 = ORIENTED_EDGE ( 'NONE', *, *, #10156, .T. ) ;
#18904 = DIRECTION ( 'NONE',  ( -0.000000000000000000, -0.000000000000000000, 1.000000000000000000 ) ) ;
#18905 = VERTEX_POINT ( 'NONE', #6185 ) ;
#18906 = DIRECTION ( 'NONE',  ( -0.9993852124581887875, 0.03505990758545896036, 0.000000000000000000 ) ) ;
#18907 = VECTOR ( 'NONE', #7866, 1000.000000000000000 ) ;
#18908 = CYLINDRICAL_SURFACE ( 'NONE', #19381, 17.50000000000000355 ) ;
#18909 = LINE ( 'NONE', #14087, #3223 ) ;
#18910 = VECTOR ( 'NONE', #6673, 1000.000000000000114 ) ;
#18911 = DIRECTION ( 'NONE',  ( -0.000000000000000000, -1.000000000000000000, -0.000000000000000000 ) ) ;
#18912 = ORIENTED_EDGE ( 'NONE', *, *, #9887, .F. ) ;
#18913 = EDGE_CURVE ( 'NONE', #20227, #7659, #332, .T. ) ;
#18914 = CARTESIAN_POINT ( 'NONE',  ( -68.18670162478832708, -38.41834839689356329, 132.4711112102474146 ) ) ;
#18915 = DIRECTION ( 'NONE',  ( -0.000000000000000000, -0.000000000000000000, 1.000000000000000000 ) ) ;
#18916 = EDGE_CURVE ( 'NONE', #17599, #19010, #5901, .T. ) ;
#18917 = EDGE_CURVE ( 'NONE', #315, #2786, #3506, .T. ) ;
#18918 = ORIENTED_EDGE ( 'NONE', *, *, #2364, .T. ) ;
#18919 = EDGE_CURVE ( 'NONE', #3127, #7889, #15694, .T. ) ;
#18920 = DIRECTION ( 'NONE',  ( 0.9749279121818223981, 0.2225209339563194444, 0.000000000000000000 ) ) ;
#18921 = CYLINDRICAL_SURFACE ( 'NONE', #16951, 9.999999999999996447 ) ;
#18922 = CARTESIAN_POINT ( 'NONE',  ( -3.143238168843667690, 31.03941509555038181, 14.88498244535547599 ) ) ;
#18923 = PLANE ( 'NONE',  #10599 ) ;
#18924 = CIRCLE ( 'NONE', #17942, 62.91752772691707207 ) ;
#18925 = CARTESIAN_POINT ( 'NONE',  ( -100.7812499999999716, -111.0996833858562809, -10.00000000000000178 ) ) ;
#18926 = CARTESIAN_POINT ( 'NONE',  ( -76.32814421828534535, 117.3631207639434564, -4.586678902943767788 ) ) ;
#18927 = VECTOR ( 'NONE', #19869, 1000.000000000000227 ) ;
#18928 = AXIS2_PLACEMENT_3D ( 'NONE', #1465, #17120, #36 ) ;
#18929 = ORIENTED_EDGE ( 'NONE', *, *, #15534, .F. ) ;
#18930 = AXIS2_PLACEMENT_3D ( 'NONE', #8983, #15436, #4286 ) ;
#18931 = DIRECTION ( 'NONE',  ( 0.1736481776669404620, -0.9848077530122062440, 0.000000000000000000 ) ) ;
#18932 = EDGE_CURVE ( 'NONE', #12045, #13334, #5058, .T. ) ;
#18933 = ORIENTED_EDGE ( 'NONE', *, *, #740, .T. ) ;
#18934 = ORIENTED_EDGE ( 'NONE', *, *, #7511, .T. ) ;
#18935 = DIRECTION ( 'NONE',  ( 0.9009688679024157043, 0.4338837391175651703, -0.000000000000000000 ) ) ;
#18936 = ORIENTED_EDGE ( 'NONE', *, *, #84, .T. ) ;
#18937 = CIRCLE ( 'NONE', #1275, 150.0000000000000284 ) ;
#18938 =( BOUNDED_SURFACE ( )  B_SPLINE_SURFACE ( 3, 2, ( 
 ( #19699, #5906, #6006 ),
 ( #13865, #2528, #1394 ),
 ( #8755, #13659, #13764 ),
 ( #4355, #7624, #10483 ),
 ( #16736, #1178, #19905 ),
 ( #10583, #2831, #5696 ),
 ( #18476, #16643, #2631 ),
 ( #4458, #8855, #20107 ),
 ( #10690, #7321, #15093 ),
 ( #9164, #11810, #18078 ),
 ( #1075, #13553, #19802 ),
 ( #18794, #9674, #1904 ),
 ( #10897, #13968, #12432 ),
 ( #7830, #1803, #7727 ),
 ( #4674, #17157, #63 ),
 ( #1498, #164, #265 ),
 ( #8138, #17051, #15921 ),
 ( #4566, #1699, #3336 ),
 ( #12638, #14385, #4778 ),
 ( #7930, #14283, #10998 ),
 ( #11202, #12533, #9576 ),
 ( #4885, #6519, #17258 ),
 ( #9271, #6315, #3236 ),
 ( #14182, #6108, #11099 ),
 ( #6214, #18897, #14075 ),
 ( #15822, #9476, #4982 ) ),
 .UNSPECIFIED., .F., .F., .F. ) 
 B_SPLINE_SURFACE_WITH_KNOTS ( ( 4, 2, 2, 2, 2, 2, 2, 2, 2, 2, 2, 2, 4 ),
 ( 3, 3 ),
 ( 0.01017271576669884214, 0.01464115812291480467, 0.01910960047913076720, 0.02134382165723874847, 0.02357804283534672973, 0.02804648519156269226, 0.03028070636967067353, 0.03251492754777865479, 0.03698336990399461732, 0.03921759108210259859, 0.04145181226021057985, 0.04368603343831856112, 0.04592025461642654238 ),
 ( 0.000000000000000000, 1.000000000000000000 ),
 .UNSPECIFIED. ) 
 GEOMETRIC_REPRESENTATION_ITEM ( )  RATIONAL_B_SPLINE_SURFACE ( (
 ( 1.000000000000000000, 0.7071067811865480168, 1.000000000000000000),
 ( 1.000000000000000000, 0.7196766872558925110, 1.000000000000000000),
 ( 1.000000000000000000, 0.7321324053394322462, 1.000000000000000000),
 ( 1.000000000000000000, 0.7567694315052313492, 1.000000000000000000),
 ( 1.000000000000000000, 0.7689510682427085353, 1.000000000000000000),
 ( 1.000000000000000000, 0.7869757430505208706, 1.000000000000000000),
 ( 1.000000000000000000, 0.7929631687998897061, 1.000000000000000000),
 ( 1.000000000000000000, 0.8046623649467963268, 1.000000000000000000),
 ( 1.000000000000000000, 0.8103917441616884654, 1.000000000000000000),
 ( 1.000000000000000000, 0.8272137286303282711, 1.000000000000000000),
 ( 1.000000000000000000, 0.8379439973090003768, 1.000000000000000000),
 ( 1.000000000000000000, 0.8532330560554670651, 1.000000000000000000),
 ( 1.000000000000000000, 0.8581942001722338009, 1.000000000000000000),
 ( 1.000000000000000000, 0.8678183107919841266, 1.000000000000000000),
 ( 1.000000000000000000, 0.8724301636763960310, 1.000000000000000000),
 ( 1.000000000000000000, 0.8855238771552775834, 1.000000000000000000),
 ( 1.000000000000000000, 0.8933247989484205398, 1.000000000000000000),
 ( 1.000000000000000000, 0.9033218449776424519, 1.000000000000000000),
 ( 1.000000000000000000, 0.9063188098300211104, 1.000000000000000000),
 ( 1.000000000000000000, 0.9115443529209835694, 1.000000000000000000),
 ( 1.000000000000000000, 0.9137831556780738884, 1.000000000000000000),
 ( 1.000000000000000000, 0.9174439670358883747, 1.000000000000000000),
 ( 1.000000000000000000, 0.9188661345742781261, 1.000000000000000000),
 ( 1.000000000000000000, 0.9207385544374218078, 1.000000000000000000),
 ( 1.000000000000000000, 0.9212071352554866976, 1.000000000000000000),
 ( 1.000000000000000000, 0.9212076576725557464, 1.000000000000000000) ) ) 
 REPRESENTATION_ITEM ( '' )  SURFACE ( )  );
#18939 = LINE ( 'NONE', #12569, #273 ) ;
#18940 = CARTESIAN_POINT ( 'NONE',  ( 29.92423416078111487, 37.80811387934369350, 248.9926560891072143 ) ) ;
#18941 = ORIENTED_EDGE ( 'NONE', *, *, #19494, .F. ) ;
#18942 = EDGE_CURVE ( 'NONE', #9222, #4680, #7553, .T. ) ;
#18943 = LINE ( 'NONE', #6458, #7349 ) ;
#18944 = CIRCLE ( 'NONE', #14983, 3.224098631618458555 ) ;
#18945 = CARTESIAN_POINT ( 'NONE',  ( 68.46530598706793569, -37.93579148621486041, 132.4711112102474146 ) ) ;
#18946 = ADVANCED_FACE ( 'NONE', ( #6689 ), #12500, .T. ) ;
#18947 = CARTESIAN_POINT ( 'NONE',  ( 0.000000000000000000, 0.000000000000000000, 40.00000000000000000 ) ) ;
#18948 = DIRECTION ( 'NONE',  ( 1.000000000000000000, 0.000000000000000000, 0.000000000000000000 ) ) ;
#18949 = ORIENTED_EDGE ( 'NONE', *, *, #19375, .T. ) ;
#18950 = CARTESIAN_POINT ( 'NONE',  ( 71.65703592476617700, -89.51573765728305432, 39.88498244535495019 ) ) ;
#18951 = DIRECTION ( 'NONE',  ( 6.982962677686266711E-15, -0.000000000000000000, 1.000000000000000000 ) ) ;
#18952 = DIRECTION ( 'NONE',  ( -0.000000000000000000, -0.000000000000000000, 1.000000000000000000 ) ) ;
#18953 = CARTESIAN_POINT ( 'NONE',  ( 103.0386482854799652, -126.0278359105729606, 38.95485802678353338 ) ) ;
#18954 = VERTEX_POINT ( 'NONE', #14147 ) ;
#18955 = CARTESIAN_POINT ( 'NONE',  ( 0.000000000000000000, 0.000000000000000000, 293.5832628385307999 ) ) ;
#18956 = CARTESIAN_POINT ( 'NONE',  ( -69.98969223978424736, 132.6704322134999074, 5.046636793514642783 ) ) ;
#18957 = ORIENTED_EDGE ( 'NONE', *, *, #13265, .T. ) ;
#18958 = VECTOR ( 'NONE', #11194, 1000.000000000000000 ) ;
#18959 = VERTEX_POINT ( 'NONE', #11174 ) ;
#18960 = ORIENTED_EDGE ( 'NONE', *, *, #14286, .T. ) ;
#18961 =( NAMED_UNIT ( * ) PLANE_ANGLE_UNIT ( ) SI_UNIT ( $, .RADIAN. ) );
#18962 = EDGE_LOOP ( 'NONE', ( #16854, #16721, #16082, #5699, #5972, #18679 ) ) ;
#18963 = CARTESIAN_POINT ( 'NONE',  ( 0.000000000000000000, 0.000000000000000000, -115.0000000000000000 ) ) ;
#18964 = CARTESIAN_POINT ( 'NONE',  ( -148.0038354016025437, 24.49305880778362976, 17.53332955362975909 ) ) ;
#18965 = ORIENTED_EDGE ( 'NONE', *, *, #9444, .F. ) ;
#18966 = LINE ( 'NONE', #16090, #15462 ) ;
#18967 = CARTESIAN_POINT ( 'NONE',  ( -73.06915264522019982, -28.06281046684251024, 111.4180192758973931 ) ) ;
#18968 = CARTESIAN_POINT ( 'NONE',  ( 50.13752642112827829, 30.53958573130925558, 132.4711112102474146 ) ) ;
#18969 = CARTESIAN_POINT ( 'NONE',  ( -96.32595581636883253, -115.9457815549233572, 29.96624877859731484 ) ) ;
#18970 = CARTESIAN_POINT ( 'NONE',  ( 77.21438937758502163, 12.78021302872874010, 248.9926560891072143 ) ) ;
#18971 = AXIS2_PLACEMENT_3D ( 'NONE', #15270, #9236, #13627 ) ;
#18972 = CARTESIAN_POINT ( 'NONE',  ( 101.0196388379316659, 100.9199429146863167, 39.99999999999999289 ) ) ;
#18973 = DIRECTION ( 'NONE',  ( -1.000000000000000000, 0.000000000000000000, 0.000000000000000000 ) ) ;
#18974 = DIRECTION ( 'NONE',  ( 0.000000000000000000, 0.000000000000000000, 1.000000000000000000 ) ) ;
#18975 = LINE ( 'NONE', #14455, #13437 ) ;
#18976 = CARTESIAN_POINT ( 'NONE',  ( 50.41613078340802190, -30.05702882063045678, 248.9926560891072143 ) ) ;
#18977 = CARTESIAN_POINT ( 'NONE',  ( -2.605298826210328045, -5.111158570922265554, 293.5832628385307999 ) ) ;
#18978 = CARTESIAN_POINT ( 'NONE',  ( -60.00000000000000000, -2.094888803305880013E-13, -100.0000000000000000 ) ) ;
#18979 = ORIENTED_EDGE ( 'NONE', *, *, #19423, .F. ) ;
#18980 = CARTESIAN_POINT ( 'NONE',  ( -124.6317628381421088, 51.51696891155003044, -26.79866528532224734 ) ) ;
#18981 = VECTOR ( 'NONE', #13533, 1000.000000000000000 ) ;
#18982 = CARTESIAN_POINT ( 'NONE',  ( -181.0783081749256382, -200.0000000000000284, 40.00000000000000000 ) ) ;
#18983 = ORIENTED_EDGE ( 'NONE', *, *, #4244, .T. ) ;
#18984 = AXIS2_PLACEMENT_3D ( 'NONE', #9573, #8231, #8331 ) ;
#18985 = EDGE_LOOP ( 'NONE', ( #16703, #15339, #15651, #17686, #17468 ) ) ;
#18986 = ORIENTED_EDGE ( 'NONE', *, *, #2197, .T. ) ;
#18987 = CARTESIAN_POINT ( 'NONE',  ( -141.6227766016837961, -18.73072656238141320, -9.999999999999985789 ) ) ;
#18988 = DIRECTION ( 'NONE',  ( -1.000000000000000000, 0.000000000000000000, 0.000000000000000000 ) ) ;
#18989 = DIRECTION ( 'NONE',  ( 1.000000000000000000, 0.000000000000000000, -0.000000000000000000 ) ) ;
#18990 = DIRECTION ( 'NONE',  ( -0.000000000000000000, -0.000000000000000000, 1.000000000000000000 ) ) ;
#18991 = EDGE_CURVE ( 'NONE', #10780, #12128, #2628, .T. ) ;
#18992 = DIRECTION ( 'NONE',  ( -1.000000000000000000, -0.000000000000000000, -0.000000000000000000 ) ) ;
#18993 = AXIS2_PLACEMENT_3D ( 'NONE', #6734, #19218, #11435 ) ;
#18994 = DIRECTION ( 'NONE',  ( 0.6234898018587442525, -0.7818314824680211439, 0.000000000000000000 ) ) ;
#18995 = DIRECTION ( 'NONE',  ( 0.000000000000000000, 0.000000000000000000, 1.000000000000000000 ) ) ;
#18996 = CARTESIAN_POINT ( 'NONE',  ( 99.98080768883885128, -130.5801677638304739, 36.60139651180438847 ) ) ;
#18997 = VECTOR ( 'NONE', #15070, 1000.000000000000000 ) ;
#18998 = CYLINDRICAL_SURFACE ( 'NONE', #1889, 62.91752772691707207 ) ;
#18999 = EDGE_LOOP ( 'NONE', ( #13611, #16803, #14880 ) ) ;
#19000 = DIRECTION ( 'NONE',  ( 0.000000000000000000, 0.000000000000000000, 1.000000000000000000 ) ) ;
#19001 = CARTESIAN_POINT ( 'NONE',  ( 134.7188131032333445, -72.93593548660993520, 30.00000000000000000 ) ) ;
#19002 = ORIENTED_EDGE ( 'NONE', *, *, #1508, .F. ) ;
#19003 = ORIENTED_EDGE ( 'NONE', *, *, #3523, .T. ) ;
#19004 = ADVANCED_FACE ( 'NONE', ( #7806 ), #16094, .T. ) ;
#19005 = ORIENTED_EDGE ( 'NONE', *, *, #14110, .F. ) ;
#19006 = EDGE_CURVE ( 'NONE', #17276, #15881, #6598, .T. ) ;
#19007 = VERTEX_POINT ( 'NONE', #11478 ) ;
#19008 = EDGE_CURVE ( 'NONE', #7363, #22, #17348, .T. ) ;
#19009 = PLANE ( 'NONE',  #1065 ) ;
#19010 = VERTEX_POINT ( 'NONE', #19648 ) ;
#19011 = CARTESIAN_POINT ( 'NONE',  ( 0.8038475772933556529, -5.196152422706607155, 8.999999999999998224 ) ) ;
#19012 = AXIS2_PLACEMENT_3D ( 'NONE', #2888, #17325, #11059 ) ;
#19013 = CARTESIAN_POINT ( 'NONE',  ( -97.77735676332854098, -133.5903492488113784, 32.35039215209604890 ) ) ;
#19014 = CARTESIAN_POINT ( 'NONE',  ( -109.9999999999983515, 285.0000000000000568, 77.50000000000000000 ) ) ;
#19015 = FACE_OUTER_BOUND ( 'NONE', #8119, .T. ) ;
#19016 = ORIENTED_EDGE ( 'NONE', *, *, #5112, .F. ) ;
#19017 = CARTESIAN_POINT ( 'NONE',  ( -15.91767397667354800, 164.0736214083062805, 60.00000000000000000 ) ) ;
#19018 = CARTESIAN_POINT ( 'NONE',  ( -4.196299268919061021, -3.911853314815648908, 293.5832628385307999 ) ) ;
#19019 = EDGE_CURVE ( 'NONE', #16017, #9870, #6789, .T. ) ;
#19020 = ORIENTED_EDGE ( 'NONE', *, *, #10006, .F. ) ;
#19021 = DIRECTION ( 'NONE',  ( -1.000000000000000000, 0.000000000000000000, 0.000000000000000000 ) ) ;
#19022 = DIRECTION ( 'NONE',  ( -0.000000000000000000, -0.000000000000000000, 1.000000000000000000 ) ) ;
#19023 = DIRECTION ( 'NONE',  ( 0.9009688679024218105, -0.4338837391175526248, 0.000000000000000000 ) ) ;
#19024 = CARTESIAN_POINT ( 'NONE',  ( 50.93469132750264095, 59.42266395395811429, 110.7293897666001214 ) ) ;
#19025 = FACE_OUTER_BOUND ( 'NONE', #14448, .T. ) ;
#19026 = CARTESIAN_POINT ( 'NONE',  ( 82.17818763663345294, -125.4865065810072622, 32.87940362201754851 ) ) ;
#19027 = ORIENTED_EDGE ( 'NONE', *, *, #4018, .T. ) ;
#19028 = CARTESIAN_POINT ( 'NONE',  ( 18.77710619359078947, 55.62246070845787216, 111.4180192758974499 ) ) ;
#19029 = AXIS2_PLACEMENT_3D ( 'NONE', #19578, #5374, #11599 ) ;
#19030 = ORIENTED_EDGE ( 'NONE', *, *, #18681, .F. ) ;
#19031 = EDGE_CURVE ( 'NONE', #12565, #11748, #10779, .T. ) ;
#19032 = VERTEX_POINT ( 'NONE', #3997 ) ;
#19033 = EDGE_CURVE ( 'NONE', #2972, #6720, #13292, .T. ) ;
#19034 = PRODUCT_DEFINITION ( 'UNKNOWN', '', #19935, #15638 ) ;
#19035 = DIRECTION ( 'NONE',  ( 0.000000000000000000, 0.000000000000000000, 1.000000000000000000 ) ) ;
#19036 = ORIENTED_EDGE ( 'NONE', *, *, #7399, .F. ) ;
#19037 = DIRECTION ( 'NONE',  ( 1.000000000000000000, 0.000000000000000000, 0.000000000000000000 ) ) ;
#19038 = DIRECTION ( 'NONE',  ( 0.9396926207859063185, -0.3420201433256742640, -6.456589605409180904E-15 ) ) ;
#19039 = ORIENTED_EDGE ( 'NONE', *, *, #16109, .T. ) ;
#19040 = DIRECTION ( 'NONE',  ( 0.000000000000000000, 0.000000000000000000, -1.000000000000000000 ) ) ;
#19041 = CARTESIAN_POINT ( 'NONE',  ( -59.42266395395758138, 50.93469132750324491, 248.9926560891072143 ) ) ;
#19042 = ADVANCED_FACE ( 'NONE', ( #14556 ), #17932, .T. ) ;
#19044 = AXIS2_PLACEMENT_3D ( 'NONE', #5777, #2036, #692 ) ;
#19043 = CARTESIAN_POINT ( 'NONE',  ( -26.42151830275515323, 4.658826548058537576, 14.88498244535563586 ) ) ;
#19045 = VECTOR ( 'NONE', #5446, 1000.000000000000000 ) ;
#19046 = PLANE ( 'NONE',  #18642 ) ;
#19047 = CARTESIAN_POINT ( 'NONE',  ( 27.90514497005375461, -110.4119590718113244, 14.88498244535525750 ) ) ;
#19048 = ORIENTED_EDGE ( 'NONE', *, *, #1724, .F. ) ;
#19049 = DIRECTION ( 'NONE',  ( -0.000000000000000000, -0.000000000000000000, 1.000000000000000000 ) ) ;
#19050 = CARTESIAN_POINT ( 'NONE',  ( 0.000000000000000000, 0.000000000000000000, -9.999999999999994671 ) ) ;
#19051 = VECTOR ( 'NONE', #15874, 1000.000000000000000 ) ;
#19052 = DIRECTION ( 'NONE',  ( 1.000000000000000000, 0.000000000000000000, -6.969309079188926949E-15 ) ) ;
#19053 = DIRECTION ( 'NONE',  ( 1.000000000000000000, 0.000000000000000000, 0.000000000000000000 ) ) ;
#19054 = ORIENTED_EDGE ( 'NONE', *, *, #1354, .T. ) ;
#19055 = LINE ( 'NONE', #1660, #8441 ) ;
#19056 = DIRECTION ( 'NONE',  ( 1.000000000000000000, 0.000000000000000000, 0.000000000000000000 ) ) ;
#19057 = EDGE_CURVE ( 'NONE', #7392, #19246, #5349, .T. ) ;
#19058 = ORIENTED_EDGE ( 'NONE', *, *, #10379, .F. ) ;
#19059 = EDGE_CURVE ( 'NONE', #4416, #9222, #17328, .T. ) ;
#19060 = ORIENTED_EDGE ( 'NONE', *, *, #14526, .T. ) ;
#19061 = EDGE_LOOP ( 'NONE', ( #18629, #15052, #2871, #19637 ) ) ;
#19062 = ITEM_DEFINED_TRANSFORMATION ( 'NONE', 'NONE', #13384,  #18639 ) ;
#19063 = VECTOR ( 'NONE', #8397, 1000.000000000000000 ) ;
#19064 = AXIS2_PLACEMENT_3D ( 'NONE', #3589, #11457, #14530 ) ;
#19065 = ORIENTED_EDGE ( 'NONE', *, *, #6523, .T. ) ;
#19066 = ADVANCED_FACE ( 'NONE', ( #7182 ), #10147, .F. ) ;
#19067 = CARTESIAN_POINT ( 'NONE',  ( -123.2437450313144893, 85.51307700781502774, 42.75112597072239851 ) ) ;
#19068 = EDGE_LOOP ( 'NONE', ( #13007, #11242, #19832, #1327 ) ) ;
#19069 = AXIS2_PLACEMENT_3D ( 'NONE', #14518, #10111, #19516 ) ;
#19070 = DIRECTION ( 'NONE',  ( 0.000000000000000000, 0.000000000000000000, 1.000000000000000000 ) ) ;
#19071 = LINE ( 'NONE', #14647, #12866 ) ;
#19072 = CARTESIAN_POINT ( 'NONE',  ( 129.2265855148630749, -76.16362387560154446, 47.28101614990461599 ) ) ;
#19073 = CARTESIAN_POINT ( 'NONE',  ( -114.7901495840402077, 80.24275698007728863, 39.74168176665586572 ) ) ;
#19074 = LINE ( 'NONE', #3415, #12470 ) ;
#19075 = VECTOR ( 'NONE', #12703, 1000.000000000000000 ) ;
#19076 = DIRECTION ( 'NONE',  ( -1.000000000000000000, 0.000000000000000000, 0.000000000000000000 ) ) ;
#19077 = FACE_OUTER_BOUND ( 'NONE', #7455, .T. ) ;
#19078 = PLANE ( 'NONE',  #7675 ) ;
#19079 = VERTEX_POINT ( 'NONE', #19271 ) ;
#19080 = CARTESIAN_POINT ( 'NONE',  ( -109.9999999999874376, 73.61623156955475622, -29.99999999999998579 ) ) ;
#19081 = AXIS2_PLACEMENT_3D ( 'NONE', #4294, #15235, #8992 ) ;
#19082 = ORIENTED_EDGE ( 'NONE', *, *, #16730, .T. ) ;
#19083 = ORIENTED_EDGE ( 'NONE', *, *, #18504, .F. ) ;
#19084 = ORIENTED_EDGE ( 'NONE', *, *, #4359, .F. ) ;
#19085 = DIRECTION ( 'NONE',  ( -0.000000000000000000, -0.000000000000000000, 1.000000000000000000 ) ) ;
#19086 = PLANE ( 'NONE',  #1102 ) ;
#19087 = CARTESIAN_POINT ( 'NONE',  ( 0.000000000000000000, 0.000000000000000000, 283.5832628385307999 ) ) ;
#19088 = VECTOR ( 'NONE', #15689, 1000.000000000000000 ) ;
#19089 = DIRECTION ( 'NONE',  ( 1.000000000000000000, 0.000000000000000000, 0.000000000000000000 ) ) ;
#19090 = DIRECTION ( 'NONE',  ( 1.000000000000000000, 0.000000000000000000, 0.000000000000000000 ) ) ;
#19091 = LINE ( 'NONE', #566, #5961 ) ;
#19092 = FACE_OUTER_BOUND ( 'NONE', #3070, .T. ) ;
#19093 = DIRECTION ( 'NONE',  ( -0.000000000000000000, -0.000000000000000000, -1.000000000000000000 ) ) ;
#19094 = PLANE ( 'NONE',  #10689 ) ;
#19095 = ORIENTED_EDGE ( 'NONE', *, *, #1271, .T. ) ;
#19096 = CARTESIAN_POINT ( 'NONE',  ( -60.00000000000000000, -2.094888803305880013E-13, -105.0000000000000142 ) ) ;
#19097 = CARTESIAN_POINT ( 'NONE',  ( 131.9720262563627386, -88.11726332927526073, 39.76694218959185179 ) ) ;
#19098 = ORIENTED_EDGE ( 'NONE', *, *, #18110, .T. ) ;
#19099 = EDGE_LOOP ( 'NONE', ( #16833, #16505 ) ) ;
#19100 = ORIENTED_EDGE ( 'NONE', *, *, #4094, .T. ) ;
#19101 = AXIS2_PLACEMENT_3D ( 'NONE', #4933, #11356, #18948 ) ;
#19102 = ORIENTED_EDGE ( 'NONE', *, *, #17243, .T. ) ;
#19103 = EDGE_CURVE ( 'NONE', #17930, #10905, #16999, .T. ) ;
#19104 = AXIS2_PLACEMENT_3D ( 'NONE', #8123, #1585, #7820 ) ;
#19105 = ORIENTED_EDGE ( 'NONE', *, *, #12893, .F. ) ;
#19106 = CARTESIAN_POINT ( 'NONE',  ( -62.91215678473957240, 0.8220851292433130064, 248.9926560891072143 ) ) ;
#19107 = CARTESIAN_POINT ( 'NONE',  ( 78.68887634719571622, -147.8252249328912740, 39.99999999999999289 ) ) ;
#19108 = DIRECTION ( 'NONE',  ( -0.5000000000000039968, 0.8660254037844363761, 0.000000000000000000 ) ) ;
#19109 = DIRECTION ( 'NONE',  ( -1.000000000000000000, 0.000000000000000000, 0.000000000000000000 ) ) ;
#19110 = VERTEX_POINT ( 'NONE', #6885 ) ;
#19111 = LINE ( 'NONE', #17684, #18790 ) ;
#19112 = DIRECTION ( 'NONE',  ( -6.982962677686266711E-15, 0.000000000000000000, -1.000000000000000000 ) ) ;
#19113 = ORIENTED_EDGE ( 'NONE', *, *, #5759, .F. ) ;
#19114 = EDGE_CURVE ( 'NONE', #19981, #6726, #640, .T. ) ;
#19115 = DIRECTION ( 'NONE',  ( 0.7660444431189707970, 0.6427876096865481337, 0.000000000000000000 ) ) ;
#19116 = PLANE ( 'NONE',  #4890 ) ;
#19117 = CIRCLE ( 'NONE', #9306, 150.0000000000000284 ) ;
#19118 = PLANE ( 'NONE',  #14724 ) ;
#19119 = EDGE_CURVE ( 'NONE', #13730, #17, #11578, .T. ) ;
#19120 = CARTESIAN_POINT ( 'NONE',  ( -56.84754764479025368, -154.7316448359455308, 60.00000000000000000 ) ) ;
#19121 = CYLINDRICAL_SURFACE ( 'NONE', #15940, 77.50000000000000000 ) ;
#19122 = DIRECTION ( 'NONE',  ( 6.982962677686266711E-15, -0.000000000000000000, 1.000000000000000000 ) ) ;
#19123 = CARTESIAN_POINT ( 'NONE',  ( 0.000000000000000000, 0.000000000000000000, 248.9926560891072143 ) ) ;
#19124 = VERTEX_POINT ( 'NONE', #13599 ) ;
#19125 = DIRECTION ( 'NONE',  ( 0.3420201433256568335, 0.9396926207859127578, 0.000000000000000000 ) ) ;
#19126 = EDGE_LOOP ( 'NONE', ( #1859, #15680, #8966 ) ) ;
#19127 = VERTEX_POINT ( 'NONE', #1024 ) ;
#19128 = EDGE_CURVE ( 'NONE', #14061, #4447, #7567, .T. ) ;
#19129 = CARTESIAN_POINT ( 'NONE',  ( 0.000000000000000000, 0.000000000000000000, 293.5832628385307999 ) ) ;
#19130 = ORIENTED_EDGE ( 'NONE', *, *, #14000, .T. ) ;
#19131 = DIRECTION ( 'NONE',  ( 1.000000000000000000, 0.000000000000000000, 0.000000000000000000 ) ) ;
#19132 = DIRECTION ( 'NONE',  ( 0.9902903945359623483, 0.1390141521205945918, 0.000000000000000000 ) ) ;
#19133 = ORIENTED_EDGE ( 'NONE', *, *, #8735, .F. ) ;
#19134 = DIRECTION ( 'NONE',  ( -6.982962677686266711E-15, 0.000000000000000000, -1.000000000000000000 ) ) ;
#19135 = FACE_OUTER_BOUND ( 'NONE', #3083, .T. ) ;
#19136 = DIRECTION ( 'NONE',  ( 6.982962677686266711E-15, -0.000000000000000000, 1.000000000000000000 ) ) ;
#19137 = EDGE_CURVE ( 'NONE', #6494, #17725, #6054, .T. ) ;
#19138 = CARTESIAN_POINT ( 'NONE',  ( 128.2779226595531270, 102.2982297021113141, 39.99999999999999289 ) ) ;
#19139 = EDGE_CURVE ( 'NONE', #5750, #17792, #10628, .T. ) ;
#19140 = CIRCLE ( 'NONE', #12251, 3.224098631618458999 ) ;
#19141 = CARTESIAN_POINT ( 'NONE',  ( -29.99999999999887379, 285.0000000000000568, 4.999999999999158007 ) ) ;
#19142 = DIRECTION ( 'NONE',  ( -0.9396926207859046531, -0.3420201433256790380, 0.000000000000000000 ) ) ;
#19143 = DIRECTION ( 'NONE',  ( -1.000000000000000000, 0.000000000000000000, 0.000000000000000000 ) ) ;
#19144 = FACE_OUTER_BOUND ( 'NONE', #10084, .T. ) ;
#19145 = DIRECTION ( 'NONE',  ( -1.000000000000000000, 0.000000000000000000, 0.000000000000000000 ) ) ;
#19146 = CARTESIAN_POINT ( 'NONE',  ( 104.7095274995394476, -123.3473593051514712, 39.62101268589415071 ) ) ;
#19147 = VERTEX_POINT ( 'NONE', #10527 ) ;
#19148 = DIRECTION ( 'NONE',  ( -0.9271237148521547233, 0.3747554100459928872, 0.000000000000000000 ) ) ;
#19149 = CARTESIAN_POINT ( 'NONE',  ( -70.15307277190674995, 132.5841624150375537, 1.385989013561256256 ) ) ;
#19150 = VERTEX_POINT ( 'NONE', #12272 ) ;
#19151 = VECTOR ( 'NONE', #5910, 1000.000000000000000 ) ;
#19152 = ORIENTED_EDGE ( 'NONE', *, *, #15905, .F. ) ;
#19153 = ORIENTED_EDGE ( 'NONE', *, *, #6787, .T. ) ;
#19154 = ADVANCED_FACE ( 'NONE', ( #18635 ), #16786, .F. ) ;
#19155 = ORIENTED_EDGE ( 'NONE', *, *, #9861, .F. ) ;
#19156 = EDGE_CURVE ( 'NONE', #5836, #14900, #4299, .T. ) ;
#19157 = CARTESIAN_POINT ( 'NONE',  ( -130.4176214210902742, 74.25971850835314569, 39.51174342451745503 ) ) ;
#19158 = EDGE_LOOP ( 'NONE', ( #17371, #17423, #10568, #11377 ) ) ;
#19159 = PRESENTATION_STYLE_ASSIGNMENT (( #17435 ) ) ;
#19160 = PLANE ( 'NONE',  #2100 ) ;
#19161 = CARTESIAN_POINT ( 'NONE',  ( -97.99247315425149907, -133.3057953413762959, 6.895088020211351143 ) ) ;
#19162 = EDGE_CURVE ( 'NONE', #9602, #10934, #12167, .T. ) ;
#19163 = ADVANCED_FACE ( 'NONE', ( #18428 ), #8461, .T. ) ;
#19165 = EDGE_CURVE ( 'NONE', #11748, #4614, #8176, .T. ) ;
#19164 = VECTOR ( 'NONE', #8847, 1000.000000000000114 ) ;
#19166 = ADVANCED_FACE ( 'NONE', ( #10738 ), #7672, .T. ) ;
#19167 = CARTESIAN_POINT ( 'NONE',  ( -137.6931958989253530, 25.38413297918773637, 26.40985621151910223 ) ) ;
#19168 = EDGE_CURVE ( 'NONE', #6419, #17764, #17668, .T. ) ;
#19169 = CARTESIAN_POINT ( 'NONE',  ( -50.13752642112849855, -30.53958573130890741, 132.4711112102474146 ) ) ;
#19170 = DIRECTION ( 'NONE',  ( -1.000000000000000000, 0.000000000000000000, 0.000000000000000000 ) ) ;
#19171 = CARTESIAN_POINT ( 'NONE',  ( -149.6969151468569237, 9.843262213762972834, -0.07667390253797667921 ) ) ;
#19172 = DIRECTION ( 'NONE',  ( 1.000000000000000000, 0.000000000000000000, 0.000000000000000000 ) ) ;
#19173 = CARTESIAN_POINT ( 'NONE',  ( -156.4179374840092862, -52.02840013024096066, 49.99999999999999289 ) ) ;
#19174 = CARTESIAN_POINT ( 'NONE',  ( 7.950000000000000178, 5.196152422706627583, 9.000000000000001776 ) ) ;
#19175 = ORIENTED_EDGE ( 'NONE', *, *, #1523, .T. ) ;
#19176 = AXIS2_PLACEMENT_3D ( 'NONE', #13867, #6215, #2832 ) ;
#19177 = DIRECTION ( 'NONE',  ( -0.000000000000000000, -1.000000000000000000, -0.000000000000000000 ) ) ;
#19178 = ORIENTED_EDGE ( 'NONE', *, *, #2630, .T. ) ;
#19179 = AXIS2_PLACEMENT_3D ( 'NONE', #7029, #19505, #5493 ) ;
#19180 = EDGE_LOOP ( 'NONE', ( #16156, #8148, #10048, #19450 ) ) ;
#19181 = VECTOR ( 'NONE', #13188, 1000.000000000000000 ) ;
#19182 = ORIENTED_EDGE ( 'NONE', *, *, #4808, .F. ) ;
#19183 = CARTESIAN_POINT ( 'NONE',  ( -110.0000000000000142, 275.0000000000000000, -75.00000000000000000 ) ) ;
#19184 = CIRCLE ( 'NONE', #12641, 7.500000000000000000 ) ;
#19185 = CARTESIAN_POINT ( 'NONE',  ( -134.9252074077219561, -65.53799637400004485, 6.377149655367134073 ) ) ;
#19186 = DIRECTION ( 'NONE',  ( -1.000000000000000000, 0.000000000000000000, 7.065055611250995019E-15 ) ) ;
#19187 = ADVANCED_FACE ( 'NONE', ( #12885 ), #6260, .T. ) ;
#19188 = CARTESIAN_POINT ( 'NONE',  ( 0.000000000000000000, -3.004629197474319246E-15, -9.000000000000000000 ) ) ;
#19189 = VERTEX_POINT ( 'NONE', #7978 ) ;
#19190 = FACE_OUTER_BOUND ( 'NONE', #12776, .T. ) ;
#19191 = CARTESIAN_POINT ( 'NONE',  ( 56.50329132715945235, -22.30005961346246579, 293.5832628385307999 ) ) ;
#19192 = DIRECTION ( 'NONE',  ( 0.000000000000000000, 0.000000000000000000, 1.000000000000000000 ) ) ;
#19193 = DIRECTION ( 'NONE',  ( 1.000000000000000000, 0.000000000000000000, 0.000000000000000000 ) ) ;
#19194 = CARTESIAN_POINT ( 'NONE',  ( -17.50000000000001066, 2.143131898507869431E-15, 293.5832628385307999 ) ) ;
#19195 = ADVANCED_FACE ( 'NONE', ( #15967 ), #19046, .F. ) ;
#19196 = ORIENTED_EDGE ( 'NONE', *, *, #16886, .F. ) ;
#19197 = CARTESIAN_POINT ( 'NONE',  ( -72.04228783541182679, 71.00759552807944885, 14.88498244535595560 ) ) ;
#19198 = VERTEX_POINT ( 'NONE', #1845 ) ;
#19200 = ORIENTED_EDGE ( 'NONE', *, *, #2349, .F. ) ;
#19199 = AXIS2_PLACEMENT_3D ( 'NONE', #8786, #20034, #5721 ) ;
#19201 = VECTOR ( 'NONE', #18669, 1000.000000000000000 ) ;
#19202 = ORIENTED_EDGE ( 'NONE', *, *, #1788, .T. ) ;
#19203 = ORIENTED_EDGE ( 'NONE', *, *, #12777, .T. ) ;
#19204 = DIRECTION ( 'NONE',  ( -0.000000000000000000, -0.000000000000000000, 1.000000000000000000 ) ) ;
#19205 = ORIENTED_EDGE ( 'NONE', *, *, #492, .F. ) ;
#19206 = LINE ( 'NONE', #2020, #12619 ) ;
#19207 = CARTESIAN_POINT ( 'NONE',  ( -100.6969204557047846, -129.5542747642292056, 37.33635527552283406 ) ) ;
#19208 = CARTESIAN_POINT ( 'NONE',  ( -18.28503710798546678, 57.92514141135458772, 293.5832628385307999 ) ) ;
#19209 = DIRECTION ( 'NONE',  ( 0.000000000000000000, 0.000000000000000000, 1.000000000000000000 ) ) ;
#19210 = ORIENTED_EDGE ( 'NONE', *, *, #12390, .F. ) ;
#19211 = CARTESIAN_POINT ( 'NONE',  ( 126.7720928841326042, -80.18313274224124143, -9.038567162788339715 ) ) ;
#19212 = DIRECTION ( 'NONE',  ( 0.9848077530122062440, 0.1736481776669404620, 0.000000000000000000 ) ) ;
#19213 = VECTOR ( 'NONE', #18911, 1000.000000000000000 ) ;
#19214 = ORIENTED_EDGE ( 'NONE', *, *, #11972, .F. ) ;
#19215 = VECTOR ( 'NONE', #8905, 1000.000000000000000 ) ;
#19216 = LINE ( 'NONE', #8254, #6105 ) ;
#19217 = FACE_OUTER_BOUND ( 'NONE', #13676, .T. ) ;
#19218 = DIRECTION ( 'NONE',  ( -6.982962677686266711E-15, 0.000000000000000000, -1.000000000000000000 ) ) ;
#19219 = EDGE_CURVE ( 'NONE', #8799, #17330, #9809, .T. ) ;
#19220 = CARTESIAN_POINT ( 'NONE',  ( -68.18670162478832708, -38.41834839689356329, 110.9660488491356887 ) ) ;
#19221 = CARTESIAN_POINT ( 'NONE',  ( -63.98537287693023501, 94.20918150411493741, 39.88498244535590231 ) ) ;
#19222 = CARTESIAN_POINT ( 'NONE',  ( -148.9554720520392834, -17.67108784863415138, 49.99999999999999289 ) ) ;
#19223 = CARTESIAN_POINT ( 'NONE',  ( 84.00455766787162304, -124.2712478689755500, 38.95858097086686200 ) ) ;
#19224 = EDGE_LOOP ( 'NONE', ( #8443, #17203, #5804, #9881, #6194, #2227 ) ) ;
#19225 = DIRECTION ( 'NONE',  ( -0.8479630283625716469, 0.5300553768524345344, 0.000000000000000000 ) ) ;
#19226 = ORIENTED_EDGE ( 'NONE', *, *, #10634, .T. ) ;
#19227 = AXIS2_PLACEMENT_3D ( 'NONE', #5789, #2715, #7610 ) ;
#19228 = ORIENTED_EDGE ( 'NONE', *, *, #10693, .T. ) ;
#19229 = DIRECTION ( 'NONE',  ( -0.000000000000000000, -0.000000000000000000, -1.000000000000000000 ) ) ;
#19230 = AXIS2_PLACEMENT_3D ( 'NONE', #8396, #4081, #16575 ) ;
#19231 = EDGE_CURVE ( 'NONE', #3673, #2735, #3483, .T. ) ;
#19232 = VERTEX_POINT ( 'NONE', #18735 ) ;
#19233 = CARTESIAN_POINT ( 'NONE',  ( 60.22232964560483737, 7.948937137877944537, 283.5832628385307999 ) ) ;
#19234 = PLANE ( 'NONE',  #10546 ) ;
#19235 = CARTESIAN_POINT ( 'NONE',  ( 0.01899995639453602378, -8.236198097127177320, -3.734486434573622393 ) ) ;
#19236 = DIRECTION ( 'NONE',  ( -6.982962677686266711E-15, 0.000000000000000000, -1.000000000000000000 ) ) ;
#19237 = CARTESIAN_POINT ( 'NONE',  ( 118.3534152657848608, 114.7431683447366595, 60.00000000000000000 ) ) ;
#19238 = CYLINDRICAL_SURFACE ( 'NONE', #1592, 60.74260934110282051 ) ;
#19239 = VECTOR ( 'NONE', #8892, 1000.000000000000000 ) ;
#19240 = VECTOR ( 'NONE', #2396, 1000.000000000000227 ) ;
#19241 = VECTOR ( 'NONE', #9292, 1000.000000000000000 ) ;
#19242 = ADVANCED_FACE ( 'NONE', ( #3183 ), #12576, .F. ) ;
#19243 = CARTESIAN_POINT ( 'NONE',  ( 0.000000000000000000, 0.000000000000000000, 60.00000000000000000 ) ) ;
#19244 = LINE ( 'NONE', #12788, #13199 ) ;
#19245 = ADVANCED_FACE ( 'NONE', ( #3385 ), #11100, .F. ) ;
#19246 = VERTEX_POINT ( 'NONE', #17408 ) ;
#19247 = CARTESIAN_POINT ( 'NONE',  ( 110.0000000000000142, 0.000000000000000000, -49.99999999999999289 ) ) ;
#19248 = DIRECTION ( 'NONE',  ( 0.000000000000000000, 0.000000000000000000, -1.000000000000000000 ) ) ;
#19249 = CARTESIAN_POINT ( 'NONE',  ( -76.83212392882499842, -14.94814811854936565, 248.9926560891072143 ) ) ;
#19250 = PLANE ( 'NONE',  #2063 ) ;
#19251 = ORIENTED_EDGE ( 'NONE', *, *, #5654, .T. ) ;
#19252 = PLANE ( 'NONE',  #17273 ) ;
#19253 = CARTESIAN_POINT ( 'NONE',  ( -79.73494653235651697, 127.0540928074882459, 31.16759418789822433 ) ) ;
#19254 = VERTEX_POINT ( 'NONE', #4823 ) ;
#19255 = EDGE_LOOP ( 'NONE', ( #9097, #10490, #19065, #8294 ) ) ;
#19256 = ORIENTED_EDGE ( 'NONE', *, *, #15498, .T. ) ;
#19257 = APPLICATION_PROTOCOL_DEFINITION ( 'draft international standard', 'automotive_design', 1998, #5678 ) ;
#19258 = EDGE_CURVE ( 'NONE', #11724, #19796, #14223, .T. ) ;
#19259 = EDGE_CURVE ( 'NONE', #18380, #13478, #2298, .T. ) ;
#19260 = VECTOR ( 'NONE', #15402, 1000.000000000000000 ) ;
#19261 = ORIENTED_EDGE ( 'NONE', *, *, #16634, .F. ) ;
#19262 = ADVANCED_FACE ( 'NONE', ( #106 ), #14016, .F. ) ;
#19263 = AXIS2_PLACEMENT_3D ( 'NONE', #11597, #15067, #17957 ) ;
#19264 = DIRECTION ( 'NONE',  ( 0.5000000000000069944, -0.8660254037844344888, 0.000000000000000000 ) ) ;
#19265 = ORIENTED_EDGE ( 'NONE', *, *, #10883, .T. ) ;
#19266 = DIRECTION ( 'NONE',  ( 0.3420201433256568335, 0.9396926207859126468, 0.000000000000000000 ) ) ;
#19267 = DIRECTION ( 'NONE',  ( 1.000000000000000000, 0.000000000000000000, 0.000000000000000000 ) ) ;
#19268 = CARTESIAN_POINT ( 'NONE',  ( -83.54968581051868171, -124.5775662629353775, 2.083218535794355120 ) ) ;
#19269 = VERTEX_POINT ( 'NONE', #11251 ) ;
#19270 = EDGE_CURVE ( 'NONE', #11697, #10402, #203, .T. ) ;
#19271 = CARTESIAN_POINT ( 'NONE',  ( -41.02212542604613787, -44.79787735033403351, 293.5832628385307999 ) ) ;
#19272 = DIRECTION ( 'NONE',  ( 1.000000000000000000, 0.000000000000000000, 0.000000000000000000 ) ) ;
#19273 = DIRECTION ( 'NONE',  ( -0.8660254037844432595, 0.4999999999999919509, -0.000000000000000000 ) ) ;
#19274 = LINE ( 'NONE', #18977, #17036 ) ;
#19275 = AXIS2_PLACEMENT_3D ( 'NONE', #10892, #17149, #3134 ) ;
#19276 = CARTESIAN_POINT ( 'NONE',  ( -110.0000000000000142, 285.0000000000000568, -75.00000000000000000 ) ) ;
#19277 = AXIS2_PLACEMENT_3D ( 'NONE', #7000, #13417, #13625 ) ;
#19278 = ORIENTED_EDGE ( 'NONE', *, *, #16159, .F. ) ;
#19279 = LINE ( 'NONE', #12614, #14771 ) ;
#19280 = VERTEX_POINT ( 'NONE', #6665 ) ;
#19281 = EDGE_CURVE ( 'NONE', #19327, #5832, #9714, .T. ) ;
#19282 = EDGE_CURVE ( 'NONE', #9602, #11122, #10834, .T. ) ;
#19283 = ORIENTED_EDGE ( 'NONE', *, *, #18884, .F. ) ;
#19284 = ADVANCED_FACE ( 'NONE', ( #4716 ), #9619, .F. ) ;
#19285 = ORIENTED_EDGE ( 'NONE', *, *, #19219, .F. ) ;
#19286 = DIRECTION ( 'NONE',  ( 1.000000000000000000, 0.000000000000000000, -6.976128451377902853E-15 ) ) ;
#19287 = CARTESIAN_POINT ( 'NONE',  ( 63.68887634719569490, -147.8252249328912740, 49.99999999999999289 ) ) ;
#19288 = DIRECTION ( 'NONE',  ( 0.5000000000000009992, -0.8660254037844380415, 0.000000000000000000 ) ) ;
#19289 = CARTESIAN_POINT ( 'NONE',  ( 0.09318607064769274251, 1.767053008364804834, -9.000000000000001776 ) ) ;
#19290 = CARTESIAN_POINT ( 'NONE',  ( -59.42266395395758138, 50.93469132750324491, 110.7293897666001214 ) ) ;
#19291 = EDGE_CURVE ( 'NONE', #18211, #19007, #1647, .T. ) ;
#19292 = DIRECTION ( 'NONE',  ( 0.000000000000000000, 0.000000000000000000, -1.000000000000000000 ) ) ;
#19293 = DIRECTION ( 'NONE',  ( 0.9396926207859046531, 0.3420201433256790380, 0.000000000000000000 ) ) ;
#19294 = CARTESIAN_POINT ( 'NONE',  ( 99.75239863728837975, -130.9022835076664535, 36.33312741211197761 ) ) ;
#19295 = LINE ( 'NONE', #8134, #8087 ) ;
#19296 = ORIENTED_EDGE ( 'NONE', *, *, #247, .T. ) ;
#19297 = CIRCLE ( 'NONE', #10142, 7.500000000000007105 ) ;
#19298 = VECTOR ( 'NONE', #14654, 1000.000000000000000 ) ;
#19299 = VERTEX_POINT ( 'NONE', #15867 ) ;
#19300 = VERTEX_POINT ( 'NONE', #6565 ) ;
#19301 = ORIENTED_EDGE ( 'NONE', *, *, #19446, .T. ) ;
#19302 = EDGE_CURVE ( 'NONE', #11985, #11567, #12787, .T. ) ;
#19303 = EDGE_CURVE ( 'NONE', #1862, #12128, #612, .T. ) ;
#19304 = EDGE_LOOP ( 'NONE', ( #14104, #5216, #11709, #9605 ) ) ;
#19305 = DIRECTION ( 'NONE',  ( 0.000000000000000000, -0.000000000000000000, 1.000000000000000000 ) ) ;
#19306 = ORIENTED_EDGE ( 'NONE', *, *, #1740, .T. ) ;
#19307 = EDGE_CURVE ( 'NONE', #15836, #15975, #19439, .T. ) ;
#19308 = DIRECTION ( 'NONE',  ( -0.9396926207859092051, 0.3420201433256662704, 0.000000000000000000 ) ) ;
#19309 = DIRECTION ( 'NONE',  ( 0.8660254037844449249, -0.4999999999999888978, 0.000000000000000000 ) ) ;
#19310 = DIRECTION ( 'NONE',  ( -0.7660444431189772363, 0.6427876096865402511, 5.380491337840974226E-15 ) ) ;
#19311 = ORIENTED_EDGE ( 'NONE', *, *, #19958, .F. ) ;
#19312 = AXIS2_PLACEMENT_3D ( 'NONE', #2257, #8486, #2058 ) ;
#19313 = LINE ( 'NONE', #14695, #12926 ) ;
#19314 = CARTESIAN_POINT ( 'NONE',  ( 62.91215678473958661, -0.8220851292428736912, 293.5832628385307999 ) ) ;
#19315 = ORIENTED_EDGE ( 'NONE', *, *, #14538, .T. ) ;
#19316 = LINE ( 'NONE', #12860, #18184 ) ;
#19317 = CARTESIAN_POINT ( 'NONE',  ( -97.59206265536059277, 66.04728469612305730, 39.88498244535613679 ) ) ;
#19318 = CARTESIAN_POINT ( 'NONE',  ( -71.18887634719365565, -147.8252249328922687, 60.00000000000000000 ) ) ;
#19319 = DIRECTION ( 'NONE',  ( 6.982962677686266711E-15, 0.000000000000000000, 1.000000000000000000 ) ) ;
#19320 = CARTESIAN_POINT ( 'NONE',  ( -23.22718332831480481, -56.12853591711337486, 283.5832628385307999 ) ) ;
#19321 = DIRECTION ( 'NONE',  ( -0.000000000000000000, -1.000000000000000000, -0.000000000000000000 ) ) ;
#19322 = ORIENTED_EDGE ( 'NONE', *, *, #13214, .F. ) ;
#19323 = CIRCLE ( 'NONE', #10469, 42.50000000000000000 ) ;
#19324 = CARTESIAN_POINT ( 'NONE',  ( 0.000000000000000000, 0.000000000000000000, 60.00000000000000000 ) ) ;
#19325 = ORIENTED_EDGE ( 'NONE', *, *, #5638, .T. ) ;
#19326 = AXIS2_PLACEMENT_3D ( 'NONE', #6693, #16097, #19172 ) ;
#19327 = VERTEX_POINT ( 'NONE', #905 ) ;
#19328 = CARTESIAN_POINT ( 'NONE',  ( 144.1955966362266679, 102.2982297021113141, 39.99999999999999289 ) ) ;
#19329 = VERTEX_POINT ( 'NONE', #12982 ) ;
#19330 = DIRECTION ( 'NONE',  ( 0.000000000000000000, 0.000000000000000000, -1.000000000000000000 ) ) ;
#19331 = FACE_OUTER_BOUND ( 'NONE', #13538, .T. ) ;
#19332 = CYLINDRICAL_SURFACE ( 'NONE', #9328, 150.0000000000000284 ) ;
#19333 = FACE_OUTER_BOUND ( 'NONE', #11562, .T. ) ;
#19334 = VERTEX_POINT ( 'NONE', #13271 ) ;
#19335 = CARTESIAN_POINT ( 'NONE',  ( -77.50000000000000000, 9.491012693391988181E-15, -115.0000000000000000 ) ) ;
#19336 = CARTESIAN_POINT ( 'NONE',  ( 99.75421581617496258, -130.9036673766147487, 3.638531688318945356 ) ) ;
#19337 = DIRECTION ( 'NONE',  ( 0.2080686897406943681, 0.9781142164131909622, 0.000000000000000000 ) ) ;
#19338 = CARTESIAN_POINT ( 'NONE',  ( -159.9599531637108782, -36.50981547337168109, 60.00000000000000000 ) ) ;
#19339 = EDGE_LOOP ( 'NONE', ( #12422, #7400, #11462 ) ) ;
#19340 = FACE_OUTER_BOUND ( 'NONE', #9015, .T. ) ;
#19341 = DIRECTION ( 'NONE',  ( 0.000000000000000000, 0.000000000000000000, 1.000000000000000000 ) ) ;
#19342 = LINE ( 'NONE', #17812, #18308 ) ;
#19343 = FACE_BOUND ( 'NONE', #19384, .T. ) ;
#19344 = EDGE_LOOP ( 'NONE', ( #3175, #7731, #1884, #6378 ) ) ;
#19345 = CARTESIAN_POINT ( 'NONE',  ( 44.79940644582654841, -41.02350267428983699, 293.5832628385307999 ) ) ;
#19346 = DIRECTION ( 'NONE',  ( 1.000000000000000000, 0.000000000000000000, 0.000000000000000000 ) ) ;
#19347 = EDGE_LOOP ( 'NONE', ( #15716, #11847, #15535, #9286 ) ) ;
#19348 = ORIENTED_EDGE ( 'NONE', *, *, #11528, .T. ) ;
#19349 = ORIENTED_EDGE ( 'NONE', *, *, #18277, .F. ) ;
#19350 = PRODUCT_CONTEXT ( 'NONE', #9854, 'mechanical' ) ;
#19351 = ADVANCED_FACE ( 'NONE', ( #11648 ), #3777, .F. ) ;
#19352 = DIRECTION ( 'NONE',  ( 0.000000000000000000, 0.000000000000000000, -1.000000000000000000 ) ) ;
#19353 = CARTESIAN_POINT ( 'NONE',  ( 32.50000000000000000, 3.980102097228897837E-15, 49.99999999999999289 ) ) ;
#19354 = ORIENTED_EDGE ( 'NONE', *, *, #5846, .F. ) ;
#19355 = AXIS2_PLACEMENT_3D ( 'NONE', #4879, #11094, #17357 ) ;
#19356 = CARTESIAN_POINT ( 'NONE',  ( 60.00000000000000711, 6.284666409917639535E-13, -115.0000000000000000 ) ) ;
#19357 = DIRECTION ( 'NONE',  ( -1.000000000000000000, 0.000000000000000000, 7.007922368489490773E-15 ) ) ;
#19358 = CARTESIAN_POINT ( 'NONE',  ( -82.84981732090430739, -125.0436758660649303, 4.143355716251761578 ) ) ;
#19359 = VERTEX_POINT ( 'NONE', #6855 ) ;
#19360 = DIRECTION ( 'NONE',  ( 6.982962677686266711E-15, -0.000000000000000000, 1.000000000000000000 ) ) ;
#19361 = CARTESIAN_POINT ( 'NONE',  ( 50.41613078340802190, -30.05702882063045678, 110.9660488491357455 ) ) ;
#19362 = EDGE_CURVE ( 'NONE', #3773, #8985, #3586, .T. ) ;
#19363 = LINE ( 'NONE', #5350, #18384 ) ;
#19364 = EDGE_CURVE ( 'NONE', #19032, #12392, #4938, .T. ) ;
#19365 =( NAMED_UNIT ( * ) SI_UNIT ( $, .STERADIAN. ) SOLID_ANGLE_UNIT ( ) );
#19366 = DIRECTION ( 'NONE',  ( -1.000000000000000000, 0.000000000000000000, 0.000000000000000000 ) ) ;
#19367 = CYLINDRICAL_SURFACE ( 'NONE', #4084, 7.500000000000020428 ) ;
#19368 = EDGE_LOOP ( 'NONE', ( #19016, #19772, #10040, #20013 ) ) ;
#19369 = EDGE_CURVE ( 'NONE', #1965, #3545, #13078, .T. ) ;
#19370 = DIRECTION ( 'NONE',  ( -6.982962677686266711E-15, 0.000000000000000000, -1.000000000000000000 ) ) ;
#19371 = CIRCLE ( 'NONE', #1049, 62.91752772691707207 ) ;
#19372 = VECTOR ( 'NONE', #2162, 1000.000000000000227 ) ;
#19373 = VECTOR ( 'NONE', #16867, 1000.000000000000000 ) ;
#19374 = ORIENTED_EDGE ( 'NONE', *, *, #3143, .F. ) ;
#19375 = EDGE_CURVE ( 'NONE', #6851, #6330, #11460, .T. ) ;
#19376 = ORIENTED_EDGE ( 'NONE', *, *, #15239, .T. ) ;
#19377 = DIRECTION ( 'NONE',  ( 0.6427876096865481337, -0.7660444431189707970, 0.000000000000000000 ) ) ;
#19378 = DIRECTION ( 'NONE',  ( -1.000000000000000000, -1.047444401652940007E-14, -0.000000000000000000 ) ) ;
#19379 = AXIS2_PLACEMENT_3D ( 'NONE', #1237, #6272, #1554 ) ;
#19380 = DIRECTION ( 'NONE',  ( 0.4999999999999978906, 0.8660254037844397068, 0.000000000000000000 ) ) ;
#19381 = AXIS2_PLACEMENT_3D ( 'NONE', #17578, #16036, #6628 ) ;
#19382 = CARTESIAN_POINT ( 'NONE',  ( 3.453261854573465683, 4.581103194070611728, 293.5832628385307999 ) ) ;
#19383 = DIRECTION ( 'NONE',  ( 0.1736481776669241417, 0.9848077530122091305, 0.000000000000000000 ) ) ;
#19384 = EDGE_LOOP ( 'NONE', ( #12437, #10857 ) ) ;
#19385 = DIRECTION ( 'NONE',  ( -6.982962677686266711E-15, 0.000000000000000000, -1.000000000000000000 ) ) ;
#19386 = CARTESIAN_POINT ( 'NONE',  ( -131.5110516633150155, -72.14693729183379389, -4.447104364459081083 ) ) ;
#19387 = EDGE_CURVE ( 'NONE', #18385, #14947, #5423, .T. ) ;
#19388 = LINE ( 'NONE', #7103, #11183 ) ;
#19389 = EDGE_CURVE ( 'NONE', #15308, #5361, #17610, .T. ) ;
#19390 = VECTOR ( 'NONE', #9807, 1000.000000000000000 ) ;
#19391 = CARTESIAN_POINT ( 'NONE',  ( 52.50000000000000711, 6.293851260911244545E-13, -105.0000000000000142 ) ) ;
#19392 = CARTESIAN_POINT ( 'NONE',  ( 8.939227532413712041, -60.08331549348429235, 293.5832628385307999 ) ) ;
#19393 = EDGE_CURVE ( 'NONE', #1887, #15200, #11741, .T. ) ;
#19394 = EDGE_LOOP ( 'NONE', ( #11644, #18851, #12368, #15622 ) ) ;
#19395 = VERTEX_POINT ( 'NONE', #11554 ) ;
#19396 = AXIS2_PLACEMENT_3D ( 'NONE', #20138, #5828, #4186 ) ;
#19397 = ORIENTED_EDGE ( 'NONE', *, *, #1653, .F. ) ;
#19398 = ORIENTED_EDGE ( 'NONE', *, *, #6650, .T. ) ;
#19399 = LINE ( 'NONE', #11609, #9921 ) ;
#19400 = EDGE_CURVE ( 'NONE', #13334, #7829, #17807, .T. ) ;
#19401 = ORIENTED_EDGE ( 'NONE', *, *, #3037, .F. ) ;
#19402 = AXIS2_PLACEMENT_3D ( 'NONE', #10276, #9042, #18158 ) ;
#19403 = DIRECTION ( 'NONE',  ( 0.000000000000000000, 0.000000000000000000, 1.000000000000000000 ) ) ;
#19404 = FACE_OUTER_BOUND ( 'NONE', #1730, .T. ) ;
#19405 = CIRCLE ( 'NONE', #775, 45.00000000000001421 ) ;
#19406 = LINE ( 'NONE', #869, #16907 ) ;
#19407 = VERTEX_POINT ( 'NONE', #10123 ) ;
#19408 = FACE_OUTER_BOUND ( 'NONE', #9976, .T. ) ;
#19409 = CARTESIAN_POINT ( 'NONE',  ( 47.56244194535165093, 37.78198917157335757, 283.5832628385307999 ) ) ;
#19410 = ORIENTED_EDGE ( 'NONE', *, *, #9541, .F. ) ;
#19411 = LINE ( 'NONE', #14992, #12373 ) ;
#19412 = CARTESIAN_POINT ( 'NONE',  ( 0.000000000000000000, 60.00000000000000000, -105.0000000000000142 ) ) ;
#19413 = LINE ( 'NONE', #2330, #3568 ) ;
#19414 = CIRCLE ( 'NONE', #784, 60.74260934110282051 ) ;
#19415 = EDGE_CURVE ( 'NONE', #10, #17163, #6571, .T. ) ;
#19416 = ADVANCED_FACE ( 'NONE', ( #13374 ), #3684, .T. ) ;
#19417 = LINE ( 'NONE', #15843, #16055 ) ;
#19418 = EDGE_CURVE ( 'NONE', #12841, #15923, #16040, .T. ) ;
#19419 = CARTESIAN_POINT ( 'NONE',  ( 138.2024300533213932, 89.85329105948596862, 60.00000000000000000 ) ) ;
#19420 = AXIS2_PLACEMENT_3D ( 'NONE', #4958, #15893, #11175 ) ;
#19421 = CARTESIAN_POINT ( 'NONE',  ( 0.000000000000000000, 0.000000000000000000, 283.5832628385307999 ) ) ;
#19422 = DIRECTION ( 'NONE',  ( 6.982962677686266711E-15, -0.000000000000000000, 1.000000000000000000 ) ) ;
#19423 = EDGE_CURVE ( 'NONE', #5032, #3673, #2324, .T. ) ;
#19424 = ORIENTED_EDGE ( 'NONE', *, *, #2388, .T. ) ;
#19425 = CARTESIAN_POINT ( 'NONE',  ( -15.91767397667355510, 149.1530343478547422, 49.99999999999999289 ) ) ;
#19426 = AXIS2_PLACEMENT_3D ( 'NONE', #2921, #7512, #10784 ) ;
#19427 = ORIENTED_EDGE ( 'NONE', *, *, #4652, .T. ) ;
#19428 = ORIENTED_EDGE ( 'NONE', *, *, #14259, .F. ) ;
#19429 = FACE_OUTER_BOUND ( 'NONE', #10346, .T. ) ;
#19430 = EDGE_LOOP ( 'NONE', ( #368, #9732, #18203, #13169 ) ) ;
#19431 = CARTESIAN_POINT ( 'NONE',  ( 7.350000000000000533, 9.000000000000000000, 0.000000000000000000 ) ) ;
#19432 = PLANE ( 'NONE',  #4704 ) ;
#19433 = STYLED_ITEM ( 'NONE', ( #4300 ), #14854 ) ;
#19434 = DIRECTION ( 'NONE',  ( -0.6427876096865430267, 0.7660444431189749048, 0.000000000000000000 ) ) ;
#19435 = CARTESIAN_POINT ( 'NONE',  ( 17.24542129382134803, 20.55229278271219329, 39.88498244535533388 ) ) ;
#19436 = ORIENTED_EDGE ( 'NONE', *, *, #13137, .F. ) ;
#19437 = DIRECTION ( 'NONE',  ( -0.3088643371590125697, 0.9511061040868803440, 0.000000000000000000 ) ) ;
#19438 = CARTESIAN_POINT ( 'NONE',  ( 98.02376510503435725, -133.2645000753678630, 6.774075666499015824 ) ) ;
#19439 = LINE ( 'NONE', #6952, #11135 ) ;
#19440 = DIRECTION ( 'NONE',  ( 0.3420201433256602197, 0.9396926207859115365, 0.000000000000000000 ) ) ;
#19441 = CARTESIAN_POINT ( 'NONE',  ( 138.2024300533213932, 89.85329105948596862, 39.99999999999999289 ) ) ;
#19442 = LINE ( 'NONE', #10216, #6454 ) ;
#19443 = CARTESIAN_POINT ( 'NONE',  ( 82.06839719201975925, -125.5578986320909678, 8.548731919517461364 ) ) ;
#19444 = AXIS2_PLACEMENT_3D ( 'NONE', #7744, #18602, #6232 ) ;
#19445 = DIRECTION ( 'NONE',  ( -1.000000000000000000, 0.000000000000000000, 0.000000000000000000 ) ) ;
#19446 = EDGE_CURVE ( 'NONE', #12253, #6115, #3308, .T. ) ;
#19447 = ORIENTED_EDGE ( 'NONE', *, *, #7977, .T. ) ;
#19448 = CARTESIAN_POINT ( 'NONE',  ( 141.8871031824808995, -16.05777877957299538, 39.99999999999999289 ) ) ;
#19449 = DIRECTION ( 'NONE',  ( -0.4693298356057531429, 0.8830229359480288309, 0.000000000000000000 ) ) ;
#19450 = ORIENTED_EDGE ( 'NONE', *, *, #18353, .T. ) ;
#19451 = VECTOR ( 'NONE', #14203, 1000.000000000000114 ) ;
#19452 = ORIENTED_EDGE ( 'NONE', *, *, #17519, .T. ) ;
#19453 = ORIENTED_EDGE ( 'NONE', *, *, #2012, .T. ) ;
#19454 = CARTESIAN_POINT ( 'NONE',  ( -76.92888220842476699, 14.39940464655786201, 132.4711112102474146 ) ) ;
#19455 = ORIENTED_EDGE ( 'NONE', *, *, #18132, .T. ) ;
#19456 = AXIS2_PLACEMENT_3D ( 'NONE', #3282, #19040, #15756 ) ;
#19457 = FACE_OUTER_BOUND ( 'NONE', #7961, .T. ) ;
#19458 = CARTESIAN_POINT ( 'NONE',  ( -97.05807359151792468, -115.6610107837965842, 10.36068692573858563 ) ) ;
#19459 = ORIENTED_EDGE ( 'NONE', *, *, #9873, .F. ) ;
#19460 = CARTESIAN_POINT ( 'NONE',  ( 67.08601213326538470, 40.32479851956839667, 110.9660488491356887 ) ) ;
#19461 =( BOUNDED_CURVE ( )  B_SPLINE_CURVE ( 3, ( #9882, #8623, #14858, #13309 ),
 .UNSPECIFIED., .F., .F. ) 
 B_SPLINE_CURVE_WITH_KNOTS ( ( 4, 4 ),
 ( 1.570796326794896336, 1.920639998745670818 ),
 .UNSPECIFIED. ) 
 CURVE ( )  GEOMETRIC_REPRESENTATION_ITEM ( )  RATIONAL_B_SPLINE_CURVE ( ( 1.000000000000000000, 0.9898267632596812193, 0.9898267632596812193, 1.000000000000000000 ) ) 
 REPRESENTATION_ITEM ( '' )  );
#19462 = LINE ( 'NONE', #7368, #5683 ) ;
#19463 = LINE ( 'NONE', #19554, #19045 ) ;
#19464 = CARTESIAN_POINT ( 'NONE',  ( -5.693982670708919613, 0.7000608949449674823, 293.5832628385307999 ) ) ;
#19465 = DIRECTION ( 'NONE',  ( -3.491481338843133355E-15, 1.000000000000000000, 0.000000000000000000 ) ) ;
#19466 = CARTESIAN_POINT ( 'NONE',  ( 49.67518383744835120, -60.47951622432767493, 248.9926560891072143 ) ) ;
#19467 = EDGE_CURVE ( 'NONE', #10138, #10141, #14722, .T. ) ;
#19468 = ORIENTED_EDGE ( 'NONE', *, *, #7253, .F. ) ;
#19469 = DIRECTION ( 'NONE',  ( -0.000000000000000000, -1.000000000000000000, -0.000000000000000000 ) ) ;
#19470 = CARTESIAN_POINT ( 'NONE',  ( 128.2779226595531270, 102.2982297021113141, 39.99999999999999289 ) ) ;
#19471 = VECTOR ( 'NONE', #10427, 999.9999999999998863 ) ;
#19472 = ORIENTED_EDGE ( 'NONE', *, *, #10019, .F. ) ;
#19473 = ORIENTED_EDGE ( 'NONE', *, *, #5875, .T. ) ;
#19474 = EDGE_CURVE ( 'NONE', #1414, #6346, #13173, .T. ) ;
#19475 = ORIENTED_EDGE ( 'NONE', *, *, #2050, .F. ) ;
#19476 = CYLINDRICAL_SURFACE ( 'NONE', #3383, 106.4288957539801004 ) ;
#19477 = VECTOR ( 'NONE', #5462, 1000.000000000000000 ) ;
#19478 = CARTESIAN_POINT ( 'NONE',  ( -110.0000000000000142, 275.0000000000000000, 5.000000000000000888 ) ) ;
#19479 = FACE_OUTER_BOUND ( 'NONE', #7012, .T. ) ;
#19480 = DIRECTION ( 'NONE',  ( 0.4999999999999916178, -0.8660254037844435926, -3.228294802704586902E-15 ) ) ;
#19481 = DIRECTION ( 'NONE',  ( -0.000000000000000000, -0.000000000000000000, 1.000000000000000000 ) ) ;
#19482 = LINE ( 'NONE', #17754, #4780 ) ;
#19483 = CARTESIAN_POINT ( 'NONE',  ( 53.78543575132128751, 32.64570716507559212, 293.5832628385307999 ) ) ;
#19484 = DIRECTION ( 'NONE',  ( 0.000000000000000000, 0.000000000000000000, 1.000000000000000000 ) ) ;
#19485 = LINE ( 'NONE', #760, #13297 ) ;
#19486 = EDGE_CURVE ( 'NONE', #5706, #12395, #20208, .T. ) ;
#19487 = VERTEX_POINT ( 'NONE', #2548 ) ;
#19488 = VECTOR ( 'NONE', #17178, 1000.000000000000114 ) ;
#19489 = ORIENTED_EDGE ( 'NONE', *, *, #19393, .T. ) ;
#19490 = CIRCLE ( 'NONE', #17860, 42.50000000000000000 ) ;
#19491 = ORIENTED_EDGE ( 'NONE', *, *, #2782, .T. ) ;
#19492 = ORIENTED_EDGE ( 'NONE', *, *, #6918, .T. ) ;
#19493 = AXIS2_PLACEMENT_3D ( 'NONE', #16946, #15407, #3139 ) ;
#19494 = EDGE_CURVE ( 'NONE', #18829, #9325, #14071, .T. ) ;
#19495 = ORIENTED_EDGE ( 'NONE', *, *, #13395, .F. ) ;
#19496 = EDGE_CURVE ( 'NONE', #9431, #15860, #8501, .T. ) ;
#19497 = DIRECTION ( 'NONE',  ( -0.9009688679024160374, -0.4338837391175646707, 0.000000000000000000 ) ) ;
#19498 = CARTESIAN_POINT ( 'NONE',  ( 60.22232964560483737, 7.948937137877944537, 293.5832628385307999 ) ) ;
#19499 = DIRECTION ( 'NONE',  ( -6.982962677686266711E-15, 0.000000000000000000, -1.000000000000000000 ) ) ;
#19500 = VERTEX_POINT ( 'NONE', #4564 ) ;
#19501 = DIRECTION ( 'NONE',  ( -0.000000000000000000, -0.000000000000000000, 1.000000000000000000 ) ) ;
#19502 = FACE_OUTER_BOUND ( 'NONE', #1657, .T. ) ;
#19503 = VERTEX_POINT ( 'NONE', #6103 ) ;
#19504 = CARTESIAN_POINT ( 'NONE',  ( 19.30071112029679625, -55.43188410062176530, 111.4180192758973362 ) ) ;
#19505 = DIRECTION ( 'NONE',  ( 0.7430374143461900838, -0.6692498792541753394, 0.000000000000000000 ) ) ;
#19506 = LINE ( 'NONE', #5494, #627 ) ;
#19507 = DIRECTION ( 'NONE',  ( -0.1736481776669340227, 0.9848077530122073542, 0.000000000000000000 ) ) ;
#19508 = AXIS2_PLACEMENT_3D ( 'NONE', #3591, #9718, #3187 ) ;
#19509 = EDGE_CURVE ( 'NONE', #3202, #20085, #15714, .T. ) ;
#19510 = CARTESIAN_POINT ( 'NONE',  ( 0.000000000000000000, 0.000000000000000000, 132.4711112102474146 ) ) ;
#19511 = CARTESIAN_POINT ( 'NONE',  ( 36.99514631729018532, -48.17959877923561862, 283.5832628385307999 ) ) ;
#19512 = ORIENTED_EDGE ( 'NONE', *, *, #6119, .F. ) ;
#19513 = DIRECTION ( 'NONE',  ( -1.000000000000000000, -0.000000000000000000, -0.000000000000000000 ) ) ;
#19514 = VERTEX_POINT ( 'NONE', #12319 ) ;
#19515 = ORIENTED_EDGE ( 'NONE', *, *, #5783, .F. ) ;
#19516 = DIRECTION ( 'NONE',  ( 0.000000000000000000, 0.000000000000000000, -1.000000000000000000 ) ) ;
#19517 = ORIENTED_EDGE ( 'NONE', *, *, #3690, .T. ) ;
#19518 = EDGE_CURVE ( 'NONE', #11442, #14900, #2313, .T. ) ;
#19519 = VECTOR ( 'NONE', #11324, 1000.000000000000000 ) ;
#19520 = EDGE_CURVE ( 'NONE', #11508, #10450, #1495, .T. ) ;
#19521 = DIRECTION ( 'NONE',  ( 6.982962677686266711E-15, -0.000000000000000000, 1.000000000000000000 ) ) ;
#19522 = VECTOR ( 'NONE', #2755, 1000.000000000000000 ) ;
#19523 = DIRECTION ( 'NONE',  ( 1.000000000000000000, 0.000000000000000000, 0.000000000000000000 ) ) ;
#19524 = DIRECTION ( 'NONE',  ( 0.000000000000000000, 0.000000000000000000, -1.000000000000000000 ) ) ;
#19525 = CARTESIAN_POINT ( 'NONE',  ( 42.44352287704987248, 94.20918150411493741, 39.88498244535516335 ) ) ;
#19526 = ORIENTED_EDGE ( 'NONE', *, *, #3109, .T. ) ;
#19527 = CARTESIAN_POINT ( 'NONE',  ( -129.8775639978177594, -75.04816271247872805, 46.61694955171623178 ) ) ;
#19528 = LINE ( 'NONE', #16272, #12699 ) ;
#19529 = CARTESIAN_POINT ( 'NONE',  ( -14.69786621328411869, 22.52834316112731017, 14.88498244535555592 ) ) ;
#19530 = CARTESIAN_POINT ( 'NONE',  ( 0.000000000000000000, 0.000000000000000000, 293.5832628385307999 ) ) ;
#19531 = EDGE_LOOP ( 'NONE', ( #1161, #16500 ) ) ;
#19532 = DIRECTION ( 'NONE',  ( -6.982962677686266711E-15, 0.000000000000000000, -1.000000000000000000 ) ) ;
#19533 = EDGE_CURVE ( 'NONE', #4430, #8683, #9472, .T. ) ;
#19534 = CARTESIAN_POINT ( 'NONE',  ( -189.9999999999988916, 285.0000000000000568, 12.50000000000027178 ) ) ;
#19535 = CARTESIAN_POINT ( 'NONE',  ( 90.16928584620099230, -119.8796671366211939, -6.536607213163578400 ) ) ;
#19536 = DIRECTION ( 'NONE',  ( 1.000000000000000000, 0.000000000000000000, 0.000000000000000000 ) ) ;
#19537 = AXIS2_PLACEMENT_3D ( 'NONE', #5484, #2514, #17974 ) ;
#19538 = ORIENTED_EDGE ( 'NONE', *, *, #16197, .T. ) ;
#19539 = AXIS2_PLACEMENT_3D ( 'NONE', #15459, #3192, #19955 ) ;
#19540 = DIRECTION ( 'NONE',  ( -0.03505990758545545621, -0.9993852124581888985, 0.000000000000000000 ) ) ;
#19541 = CARTESIAN_POINT ( 'NONE',  ( 23.22641211976290876, 56.12662799072082720, 283.5832628385307999 ) ) ;
#19542 = EDGE_LOOP ( 'NONE', ( #1064, #7914, #3864, #963 ) ) ;
#19543 = ORIENTED_EDGE ( 'NONE', *, *, #13785, .T. ) ;
#19544 = EDGE_CURVE ( 'NONE', #7600, #19595, #2966, .T. ) ;
#19545 = CARTESIAN_POINT ( 'NONE',  ( 0.000000000000000000, 0.000000000000000000, 283.5832628385307999 ) ) ;
#19546 = ORIENTED_EDGE ( 'NONE', *, *, #19128, .T. ) ;
#19547 = CARTESIAN_POINT ( 'NONE',  ( 93.96728894854133785, -116.9213660262077781, -8.642061447020635612 ) ) ;
#19548 = CARTESIAN_POINT ( 'NONE',  ( -99.15855529360358389, -131.7281685730150684, 4.481768808781215085 ) ) ;
#19549 = AXIS2_PLACEMENT_3D ( 'NONE', #6997, #8628, #6805 ) ;
#19550 = VECTOR ( 'NONE', #14916, 1000.000000000000227 ) ;
#19551 = EDGE_CURVE ( 'NONE', #15057, #8591, #59, .T. ) ;
#19552 = AXIS2_PLACEMENT_3D ( 'NONE', #13382, #8688, #3891 ) ;
#19553 = CARTESIAN_POINT ( 'NONE',  ( -88.72241907111768455, -120.9490000788567130, -5.329395631252526577 ) ) ;
#19554 = CARTESIAN_POINT ( 'NONE',  ( 63.68887634719569490, -147.8252249328912740, 60.00000000000000000 ) ) ;
#19555 = DIRECTION ( 'NONE',  ( 0.4999999999999888978, 0.8660254037844449249, 0.000000000000000000 ) ) ;
#19556 = CARTESIAN_POINT ( 'NONE',  ( 71.18887634719571622, -147.8252249328912740, 60.00000000000000000 ) ) ;
#19557 = CARTESIAN_POINT ( 'NONE',  ( 0.000000000000000000, 0.000000000000000000, 248.9926560891072143 ) ) ;
#19558 = VERTEX_POINT ( 'NONE', #19624 ) ;
#19559 = FACE_OUTER_BOUND ( 'NONE', #16894, .T. ) ;
#19560 = LINE ( 'NONE', #7190, #2367 ) ;
#19561 = VECTOR ( 'NONE', #5927, 1000.000000000000000 ) ;
#19562 = AXIS2_PLACEMENT_3D ( 'NONE', #7127, #7223, #5692 ) ;
#19563 = VERTEX_POINT ( 'NONE', #9161 ) ;
#19564 = ORIENTED_EDGE ( 'NONE', *, *, #19885, .F. ) ;
#19565 = LINE ( 'NONE', #5557, #6090 ) ;
#19566 = ORIENTED_EDGE ( 'NONE', *, *, #8971, .F. ) ;
#19567 = CARTESIAN_POINT ( 'NONE',  ( 134.7088403748421399, -73.01573503433813528, 9.021076383413966226 ) ) ;
#19568 = VECTOR ( 'NONE', #17733, 1000.000000000000000 ) ;
#19569 =( BOUNDED_CURVE ( )  B_SPLINE_CURVE ( 3, ( #9160, #18582, #18690, #13861 ),
 .UNSPECIFIED., .F., .F. ) 
 B_SPLINE_CURVE_WITH_KNOTS ( ( 4, 4 ),
 ( -1.776356839400250465E-15, 1.570796326794896336 ),
 .UNSPECIFIED. ) 
 CURVE ( )  GEOMETRIC_REPRESENTATION_ITEM ( )  RATIONAL_B_SPLINE_CURVE ( ( 1.000000000000000000, 0.8047378541243646044, 0.8047378541243646044, 1.000000000000000000 ) ) 
 REPRESENTATION_ITEM ( '' )  );
#19570 = CARTESIAN_POINT ( 'NONE',  ( -133.3415482518558122, -68.70949856429524516, -0.7195383986325173398 ) ) ;
#19571 = CARTESIAN_POINT ( 'NONE',  ( -7.500000000000006217, 164.0736214083062805, 39.99999999999999289 ) ) ;
#19572 = DIRECTION ( 'NONE',  ( -0.9993852124581887875, 0.03505990758545896036, 0.000000000000000000 ) ) ;
#19573 = AXIS2_PLACEMENT_3D ( 'NONE', #13592, #1329, #8991 ) ;
#19574 = VECTOR ( 'NONE', #8455, 1000.000000000000000 ) ;
#19575 = ORIENTED_EDGE ( 'NONE', *, *, #7007, .T. ) ;
#19576 = CARTESIAN_POINT ( 'NONE',  ( 0.000000000000000000, 0.000000000000000000, 0.000000000000000000 ) ) ;
#19577 = CARTESIAN_POINT ( 'NONE',  ( -132.7526696464364875, -84.67545766722497547, 0.8872275965778846363 ) ) ;
#19578 = CARTESIAN_POINT ( 'NONE',  ( 113.5802308907677372, 8.308367629983374414, 39.88498244535465886 ) ) ;
#19579 = CARTESIAN_POINT ( 'NONE',  ( 10.11498556985161024, -62.09913334491128012, 248.9926560891072143 ) ) ;
#19580 = CARTESIAN_POINT ( 'NONE',  ( 60.08331549348424971, 8.939227532413909216, 293.5832628385307999 ) ) ;
#19581 = CARTESIAN_POINT ( 'NONE',  ( -134.5816389422690236, -73.99824545063825099, 33.10625479714592956 ) ) ;
#19582 = ORIENTED_EDGE ( 'NONE', *, *, #7705, .F. ) ;
#19583 = EDGE_LOOP ( 'NONE', ( #18099, #11611, #19428, #3765 ) ) ;
#19584 = EDGE_LOOP ( 'NONE', ( #6048, #13536, #8195, #15980 ) ) ;
#19585 = AXIS2_PLACEMENT_3D ( 'NONE', #11948, #10424, #3278 ) ;
#19586 = VECTOR ( 'NONE', #10449, 1000.000000000000000 ) ;
#19587 = ORIENTED_EDGE ( 'NONE', *, *, #6746, .F. ) ;
#19588 = ORIENTED_EDGE ( 'NONE', *, *, #3602, .F. ) ;
#19589 = EDGE_CURVE ( 'NONE', #19198, #3495, #4672, .T. ) ;
#19590 = DIRECTION ( 'NONE',  ( 0.9848077530122085754, -0.1736481776669273336, 0.000000000000000000 ) ) ;
#19591 = DIRECTION ( 'NONE',  ( -0.6427876096865300370, -0.7660444431189858960, 0.000000000000000000 ) ) ;
#19592 = ORIENTED_EDGE ( 'NONE', *, *, #19904, .T. ) ;
#19593 = DIRECTION ( 'NONE',  ( 0.000000000000000000, 0.000000000000000000, 1.000000000000000000 ) ) ;
#19594 = CARTESIAN_POINT ( 'NONE',  ( -62.18629025319808790, 9.564549117045718418, 132.4711112102474146 ) ) ;
#19595 = VERTEX_POINT ( 'NONE', #6313 ) ;
#19596 = ADVANCED_FACE ( 'NONE', ( #11931 ), #16943, .T. ) ;
#19597 = DIRECTION ( 'NONE',  ( 1.000000000000000000, 0.000000000000000000, 0.000000000000000000 ) ) ;
#19598 = DIRECTION ( 'NONE',  ( 0.000000000000000000, 0.000000000000000000, -1.000000000000000000 ) ) ;
#19599 = CARTESIAN_POINT ( 'NONE',  ( 3.911853314815638694, -4.196299268919047698, 293.5832628385307999 ) ) ;
#19600 = AXIS2_PLACEMENT_3D ( 'NONE', #15573, #10647, #15776 ) ;
#19601 = CIRCLE ( 'NONE', #3919, 7.500000000000008882 ) ;
#19602 = DIRECTION ( 'NONE',  ( -1.000000000000000000, 0.000000000000000000, 0.000000000000000000 ) ) ;
#19603 = EDGE_CURVE ( 'NONE', #20212, #5133, #12530, .T. ) ;
#19604 = EDGE_CURVE ( 'NONE', #625, #12873, #15045, .T. ) ;
#19605 = DIRECTION ( 'NONE',  ( 1.000000000000000000, 0.000000000000000000, 0.000000000000000000 ) ) ;
#19606 = CARTESIAN_POINT ( 'NONE',  ( -77.21438937758512111, -12.78021302872824094, 132.4711112102474146 ) ) ;
#19607 = ORIENTED_EDGE ( 'NONE', *, *, #17778, .T. ) ;
#19608 = EDGE_CURVE ( 'NONE', #18849, #15505, #18097, .T. ) ;
#19609 = CARTESIAN_POINT ( 'NONE',  ( 0.5595136366802733185, -4.349754824395939856, -8.999999999999998224 ) ) ;
#19610 = VERTEX_POINT ( 'NONE', #7827 ) ;
#19611 = EDGE_LOOP ( 'NONE', ( #19182, #17760, #10917, #4083 ) ) ;
#19612 = CARTESIAN_POINT ( 'NONE',  ( 30.74413178637192701, -54.89456854707552935, 293.5832628385307999 ) ) ;
#19613 = ORIENTED_EDGE ( 'NONE', *, *, #9143, .T. ) ;
#19614 = ORIENTED_EDGE ( 'NONE', *, *, #272, .F. ) ;
#19615 = AXIS2_PLACEMENT_3D ( 'NONE', #8382, #709, #5230 ) ;
#19616 = ADVANCED_FACE ( 'NONE', ( #18789 ), #11834, .T. ) ;
#19617 = FACE_OUTER_BOUND ( 'NONE', #17263, .T. ) ;
#19618 = CARTESIAN_POINT ( 'NONE',  ( -5.111158570922240685, 2.605298826210305840, 293.5832628385307999 ) ) ;
#19619 = DIRECTION ( 'NONE',  ( 0.000000000000000000, 0.000000000000000000, 1.000000000000000000 ) ) ;
#19620 = LINE ( 'NONE', #16660, #15523 ) ;
#19621 = VERTEX_POINT ( 'NONE', #16119 ) ;
#19622 = LINE ( 'NONE', #18094, #16242 ) ;
#19623 = DIRECTION ( 'NONE',  ( 0.000000000000000000, 0.000000000000000000, -1.000000000000000000 ) ) ;
#19624 = CARTESIAN_POINT ( 'NONE',  ( 100.5989061668482520, 55.02415981988612970, 14.88498244535475123 ) ) ;
#19625 = CARTESIAN_POINT ( 'NONE',  ( 3.221721112346273674, 26.70531838198836283, 14.88498244535543158 ) ) ;
#19626 = CIRCLE ( 'NONE', #5275, 9.000000000000000000 ) ;
#19627 = EDGE_LOOP ( 'NONE', ( #14464, #6845, #5803, #15593 ) ) ;
#19628 = LINE ( 'NONE', #13082, #7730 ) ;
#19629 = ADVANCED_FACE ( 'NONE', ( #466, #1799 ), #259, .F. ) ;
#19630 = CARTESIAN_POINT ( 'NONE',  ( 84.98223365279407915, -123.6049511534864536, -0.7930668616445250008 ) ) ;
#19631 = AXIS2_PLACEMENT_3D ( 'NONE', #10973, #13631, #12505 ) ;
#19632 = PLANE ( 'NONE',  #17080 ) ;
#19633 = ORIENTED_EDGE ( 'NONE', *, *, #4544, .T. ) ;
#19634 = EDGE_CURVE ( 'NONE', #3485, #4464, #17683, .T. ) ;
#19635 = DIRECTION ( 'NONE',  ( 0.000000000000000000, 0.000000000000000000, 1.000000000000000000 ) ) ;
#19636 = FACE_OUTER_BOUND ( 'NONE', #1890, .T. ) ;
#19637 = ORIENTED_EDGE ( 'NONE', *, *, #9659, .T. ) ;
#19638 = VERTEX_POINT ( 'NONE', #6712 ) ;
#19639 = AXIS2_PLACEMENT_3D ( 'NONE', #7810, #2809, #7598 ) ;
#19640 = VERTEX_POINT ( 'NONE', #357 ) ;
#19641 = LINE ( 'NONE', #4191, #16645 ) ;
#19642 = AXIS2_PLACEMENT_3D ( 'NONE', #2776, #16992, #9104 ) ;
#19643 = ADVANCED_FACE ( 'NONE', ( #12934 ), #11411, .F. ) ;
#19644 = DIRECTION ( 'NONE',  ( 1.000000000000000000, 0.000000000000000000, 0.000000000000000000 ) ) ;
#19645 = ORIENTED_EDGE ( 'NONE', *, *, #13655, .T. ) ;
#19646 = PLANE ( 'NONE',  #8343 ) ;
#19647 = CARTESIAN_POINT ( 'NONE',  ( 2.629250726500717672, 60.68567895461850270, 293.5832628385307999 ) ) ;
#19648 = CARTESIAN_POINT ( 'NONE',  ( 7.500000000000006217, 164.0736214083062805, 39.99999999999999289 ) ) ;
#19649 = LINE ( 'NONE', #5642, #17039 ) ;
#19650 = DIRECTION ( 'NONE',  ( 0.6234898018587442525, -0.7818314824680211439, 0.000000000000000000 ) ) ;
#19651 = EDGE_CURVE ( 'NONE', #3485, #20118, #14179, .T. ) ;
#19652 = CARTESIAN_POINT ( 'NONE',  ( -60.83768308848344475, 49.24833719034248958, 248.9926560891072143 ) ) ;
#19653 = DIRECTION ( 'NONE',  ( -0.7660444431189858960, -0.6427876096865299260, 5.346191897317643224E-15 ) ) ;
#19654 = ADVANCED_FACE ( 'NONE', ( #14278 ), #12096, .T. ) ;
#19655 = EDGE_LOOP ( 'NONE', ( #8650, #299, #16378, #8470 ) ) ;
#19656 = LINE ( 'NONE', #15053, #5492 ) ;
#19657 = DIRECTION ( 'NONE',  ( 0.000000000000000000, 0.000000000000000000, -1.000000000000000000 ) ) ;
#19658 = EDGE_LOOP ( 'NONE', ( #4032, #18831, #17949, #12007 ) ) ;
#19659 = ADVANCED_FACE ( 'NONE', ( #11199 ), #17663, .F. ) ;
#19660 = ORIENTED_EDGE ( 'NONE', *, *, #3964, .T. ) ;
#19661 = CIRCLE ( 'NONE', #1036, 7.500000000000003553 ) ;
#19662 = ORIENTED_EDGE ( 'NONE', *, *, #11308, .F. ) ;
#19663 = LINE ( 'NONE', #8717, #3161 ) ;
#19664 = VERTEX_POINT ( 'NONE', #12735 ) ;
#19665 = CARTESIAN_POINT ( 'NONE',  ( 79.05640494598117129, -127.4758205975433327, 60.00000000000000000 ) ) ;
#19666 = DIRECTION ( 'NONE',  ( -0.4999999999999950040, -0.8660254037844415942, 0.000000000000000000 ) ) ;
#19667 = DIRECTION ( 'NONE',  ( 0.000000000000000000, 0.000000000000000000, 1.000000000000000000 ) ) ;
#19668 = ADVANCED_BREP_SHAPE_REPRESENTATION ( '', ( #8228, #18639 ), #3610 ) ;
#19669 = CARTESIAN_POINT ( 'NONE',  ( -67.50000000000000000, -2.085703952312275003E-13, -115.0000000000000000 ) ) ;
#19670 = DIRECTION ( 'NONE',  ( -6.982962677686266711E-15, 0.000000000000000000, -1.000000000000000000 ) ) ;
#19671 = CARTESIAN_POINT ( 'NONE',  ( 0.000000000000000000, 0.000000000000000000, -105.0000000000000142 ) ) ;
#19672 = EDGE_LOOP ( 'NONE', ( #5996, #16553, #6242, #5474 ) ) ;
#19673 = FACE_OUTER_BOUND ( 'NONE', #1219, .T. ) ;
#19674 = CARTESIAN_POINT ( 'NONE',  ( -126.7530218919690412, -80.25302646196961120, -0.9824221781708450951 ) ) ;
#19675 = CARTESIAN_POINT ( 'NONE',  ( 133.2712073793125285, -68.96827650305598922, 10.00000000000000711 ) ) ;
#19676 = VECTOR ( 'NONE', #9750, 1000.000000000000114 ) ;
#19677 = AXIS2_PLACEMENT_3D ( 'NONE', #17514, #14019, #1746 ) ;
#19678 = FACE_OUTER_BOUND ( 'NONE', #4916, .T. ) ;
#19679 = CARTESIAN_POINT ( 'NONE',  ( -110.0000000000000142, 265.0000000000000000, 44.99999999999998579 ) ) ;
#19680 = ORIENTED_EDGE ( 'NONE', *, *, #4212, .F. ) ;
#19681 = AXIS2_PLACEMENT_3D ( 'NONE', #11387, #2089, #2679 ) ;
#19682 = ORIENTED_EDGE ( 'NONE', *, *, #10622, .T. ) ;
#19683 = VERTEX_POINT ( 'NONE', #1899 ) ;
#19684 = ORIENTED_EDGE ( 'NONE', *, *, #14892, .T. ) ;
#19685 = VECTOR ( 'NONE', #1450, 1000.000000000000000 ) ;
#19686 = AXIS2_PLACEMENT_3D ( 'NONE', #1357, #18443, #4422 ) ;
#19687 = ORIENTED_EDGE ( 'NONE', *, *, #5367, .T. ) ;
#19688 = DIRECTION ( 'NONE',  ( 6.982962677686266711E-15, -0.000000000000000000, 1.000000000000000000 ) ) ;
#19689 = DIRECTION ( 'NONE',  ( 0.000000000000000000, 0.000000000000000000, -1.000000000000000000 ) ) ;
#19690 = ORIENTED_EDGE ( 'NONE', *, *, #18916, .F. ) ;
#19691 = VECTOR ( 'NONE', #18803, 1000.000000000000227 ) ;
#19692 = CYLINDRICAL_SURFACE ( 'NONE', #11625, 62.91752772691707207 ) ;
#19693 = DIRECTION ( 'NONE',  ( 1.000000000000000000, 0.000000000000000000, 0.000000000000000000 ) ) ;
#19694 = ORIENTED_EDGE ( 'NONE', *, *, #2142, .F. ) ;
#19695 = DIRECTION ( 'NONE',  ( -0.000000000000000000, -0.000000000000000000, 1.000000000000000000 ) ) ;
#19696 = CARTESIAN_POINT ( 'NONE',  ( 141.8714406926368099, -48.70825716237079916, 39.99999999999999289 ) ) ;
#19697 = CARTESIAN_POINT ( 'NONE',  ( -131.9720262563626818, -88.11726332927524652, 0.2330578104081588442 ) ) ;
#19698 = DIRECTION ( 'NONE',  ( -0.7430374143461878633, 0.6692498792541777819, 0.000000000000000000 ) ) ;
#19699 = CARTESIAN_POINT ( 'NONE',  ( 122.8001410695374886, -86.14014948502062907, 50.00000000000000000 ) ) ;
#19700 = VERTEX_POINT ( 'NONE', #4881 ) ;
#19701 = EDGE_CURVE ( 'NONE', #8834, #6452, #568, .T. ) ;
#19702 = DIRECTION ( 'NONE',  ( -1.000000000000000000, 0.000000000000000000, 0.000000000000000000 ) ) ;
#19703 = VERTEX_POINT ( 'NONE', #8031 ) ;
#19704 = VECTOR ( 'NONE', #10178, 1000.000000000000000 ) ;
#19705 = ORIENTED_EDGE ( 'NONE', *, *, #17560, .T. ) ;
#19706 = CARTESIAN_POINT ( 'NONE',  ( 28.06680738835026290, -53.87178215532764369, 283.5832628385307999 ) ) ;
#19707 = AXIS2_PLACEMENT_3D ( 'NONE', #177, #9685, #6228 ) ;
#19708 = EDGE_LOOP ( 'NONE', ( #10843, #18513, #18487, #11841 ) ) ;
#19709 = ORIENTED_EDGE ( 'NONE', *, *, #3956, .F. ) ;
#19710 = FACE_OUTER_BOUND ( 'NONE', #8599, .T. ) ;
#19711 = EDGE_CURVE ( 'NONE', #16974, #13478, #4860, .T. ) ;
#19712 = DIRECTION ( 'NONE',  ( 0.3420201433256631063, 0.9396926207859105373, 0.000000000000000000 ) ) ;
#19713 = CARTESIAN_POINT ( 'NONE',  ( 0.09252763182292092492, 8.674330214978045461, 2.975619346028168355 ) ) ;
#19714 = CARTESIAN_POINT ( 'NONE',  ( 0.000000000000000000, 0.000000000000000000, 248.9926560891072143 ) ) ;
#19715 = CYLINDRICAL_SURFACE ( 'NONE', #10281, 7.500000000000007105 ) ;
#19716 = EDGE_CURVE ( 'NONE', #17433, #18511, #12757, .T. ) ;
#19717 = VERTEX_POINT ( 'NONE', #19391 ) ;
#19718 = CARTESIAN_POINT ( 'NONE',  ( -133.9144309718294892, -67.58001956112551056, 38.90204870918451263 ) ) ;
#19719 = FACE_OUTER_BOUND ( 'NONE', #16239, .T. ) ;
#19720 = VECTOR ( 'NONE', #329, 1000.000000000000114 ) ;
#19721 = DIRECTION ( 'NONE',  ( 6.982962677686266711E-15, -0.000000000000000000, 1.000000000000000000 ) ) ;
#19722 = CARTESIAN_POINT ( 'NONE',  ( -51.36153797460868731, 59.06449708980215263, 110.7293897666001214 ) ) ;
#19723 = ORIENTED_EDGE ( 'NONE', *, *, #3840, .T. ) ;
#19724 = VECTOR ( 'NONE', #8741, 1000.000000000000114 ) ;
#19725 = FACE_OUTER_BOUND ( 'NONE', #9208, .T. ) ;
#19726 = CARTESIAN_POINT ( 'NONE',  ( -130.9868171408399462, -91.88282611735537841, 40.00000000000000000 ) ) ;
#19727 = FACE_OUTER_BOUND ( 'NONE', #18015, .T. ) ;
#19728 = ORIENTED_EDGE ( 'NONE', *, *, #1015, .F. ) ;
#19729 = ADVANCED_FACE ( 'NONE', ( #14967 ), #13122, .F. ) ;
#19730 = CARTESIAN_POINT ( 'NONE',  ( -12.14914984460759761, -59.51523122377249564, 293.5832628385307999 ) ) ;
#19731 = CARTESIAN_POINT ( 'NONE',  ( 159.9599531637113330, -36.50981547336952104, 39.99999999999999289 ) ) ;
#19732 = ORIENTED_EDGE ( 'NONE', *, *, #8415, .T. ) ;
#19733 = ORIENTED_EDGE ( 'NONE', *, *, #9143, .F. ) ;
#19734 = CARTESIAN_POINT ( 'NONE',  ( -96.95682486762434849, -115.7027609144189597, 29.61261940427053929 ) ) ;
#19735 = CIRCLE ( 'NONE', #9951, 3.224098631618460775 ) ;
#19736 = ORIENTED_EDGE ( 'NONE', *, *, #2883, .T. ) ;
#19737 = CYLINDRICAL_SURFACE ( 'NONE', #645, 9.999999999999994671 ) ;
#19738 = ADVANCED_FACE ( 'NONE', ( #7104 ), #17960, .F. ) ;
#19739 = LINE ( 'NONE', #19454, #11960 ) ;
#19740 = CIRCLE ( 'NONE', #13527, 99.99999999999997158 ) ;
#19741 = ORIENTED_EDGE ( 'NONE', *, *, #10990, .F. ) ;
#19742 = ADVANCED_FACE ( 'NONE', ( #5569 ), #11888, .T. ) ;
#19743 = CARTESIAN_POINT ( 'NONE',  ( 100.7812500000000284, -111.0996833858562809, -3.469446951953614189E-15 ) ) ;
#19744 = CARTESIAN_POINT ( 'NONE',  ( 167.4599531637113330, -36.50981547336952104, 60.00000000000000000 ) ) ;
#19745 = ADVANCED_FACE ( 'NONE', ( #2604 ), #10265, .T. ) ;
#19746 = VECTOR ( 'NONE', #6433, 1000.000000000000000 ) ;
#19747 = DIRECTION ( 'NONE',  ( 0.000000000000000000, 0.000000000000000000, -1.000000000000000000 ) ) ;
#19748 = DIRECTION ( 'NONE',  ( -0.000000000000000000, -0.000000000000000000, 1.000000000000000000 ) ) ;
#19749 = LINE ( 'NONE', #13398, #15827 ) ;
#19750 = CARTESIAN_POINT ( 'NONE',  ( 44.79940644582654841, -41.02350267428983699, 283.5832628385307999 ) ) ;
#19751 = DIRECTION ( 'NONE',  ( -0.000000000000000000, -0.000000000000000000, -1.000000000000000000 ) ) ;
#19752 = CARTESIAN_POINT ( 'NONE',  ( -50.93469132750304595, -59.42266395395774481, 110.7293897666001214 ) ) ;
#19753 = ORIENTED_EDGE ( 'NONE', *, *, #1201, .T. ) ;
#19754 = EDGE_CURVE ( 'NONE', #12482, #19664, #7537, .T. ) ;
#19755 = DIRECTION ( 'NONE',  ( 0.9749279121818261729, -0.2225209339563031519, 0.000000000000000000 ) ) ;
#19756 = CARTESIAN_POINT ( 'NONE',  ( -2.300765332208364988, -116.0870680293436408, 14.88498244535546711 ) ) ;
#19757 = EDGE_LOOP ( 'NONE', ( #19761, #8982, #4465, #8866 ) ) ;
#19758 = ORIENTED_EDGE ( 'NONE', *, *, #3641, .T. ) ;
#19759 = SHAPE_REPRESENTATION_RELATIONSHIP ( 'NONE' , 'NONE' ,  #16185, #8694 ) ;
#19760 = VECTOR ( 'NONE', #19818, 1000.000000000000000 ) ;
#19761 = ORIENTED_EDGE ( 'NONE', *, *, #493, .F. ) ;
#19762 = CARTESIAN_POINT ( 'NONE',  ( 0.000000000000000000, 0.000000000000000000, 49.99999999999999289 ) ) ;
#19763 = VERTEX_POINT ( 'NONE', #13224 ) ;
#19764 = CIRCLE ( 'NONE', #19681, 3.224098631618458999 ) ;
#19765 = EDGE_CURVE ( 'NONE', #14077, #22, #10170, .T. ) ;
#19766 = CARTESIAN_POINT ( 'NONE',  ( 133.6084294554693770, -80.28749220512219154, 2.341744974304089233 ) ) ;
#19767 = EDGE_CURVE ( 'NONE', #13329, #18614, #17373, .T. ) ;
#19768 = CARTESIAN_POINT ( 'NONE',  ( 28.94983032429829350, -53.40245231972188833, 283.5832628385307999 ) ) ;
#19769 = CARTESIAN_POINT ( 'NONE',  ( -100.7812499999999716, -111.0996833858563093, 40.00000000000001421 ) ) ;
#19770 = CARTESIAN_POINT ( 'NONE',  ( -5.729042578294415655, -0.2993243175132198064, 293.5832628385307999 ) ) ;
#19771 = DIRECTION ( 'NONE',  ( -0.9511061040868794558, -0.3088643371590157338, 0.000000000000000000 ) ) ;
#19772 = ORIENTED_EDGE ( 'NONE', *, *, #506, .T. ) ;
#19773 = DIRECTION ( 'NONE',  ( 0.000000000000000000, 0.000000000000000000, 1.000000000000000000 ) ) ;
#19774 = FACE_BOUND ( 'NONE', #18621, .T. ) ;
#19775 = CARTESIAN_POINT ( 'NONE',  ( 125.5830613944035576, -82.05591916721346024, -1.021718221178191222 ) ) ;
#19776 = DIRECTION ( 'NONE',  ( 1.000000000000000000, 0.000000000000000000, 0.000000000000000000 ) ) ;
#19777 = CARTESIAN_POINT ( 'NONE',  ( 97.50000000000002842, -189.9999999999999716, 40.00000000000000000 ) ) ;
#19778 = FACE_OUTER_BOUND ( 'NONE', #6992, .T. ) ;
#19779 = EDGE_LOOP ( 'NONE', ( #17324, #1858, #68, #16349, #4460, #19526 ) ) ;
#19780 = ADVANCED_FACE ( 'NONE', ( #14870 ), #10073, .F. ) ;
#19781 = LINE ( 'NONE', #1055, #7579 ) ;
#19782 = ORIENTED_EDGE ( 'NONE', *, *, #1426, .F. ) ;
#19783 = VERTEX_POINT ( 'NONE', #19579 ) ;
#19784 = VECTOR ( 'NONE', #2424, 1000.000000000000000 ) ;
#19785 = EDGE_LOOP ( 'NONE', ( #13638, #12126, #19705, #16742 ) ) ;
#19786 = ORIENTED_EDGE ( 'NONE', *, *, #19415, .F. ) ;
#19787 = ADVANCED_FACE ( 'NONE', ( #14773 ), #8437, .T. ) ;
#19788 = CARTESIAN_POINT ( 'NONE',  ( -1.379293853801755176, 62.90240729679781850, 248.9926560891072143 ) ) ;
#19789 = AXIS2_PLACEMENT_3D ( 'NONE', #15238, #9099, #1225 ) ;
#19790 = LINE ( 'NONE', #19987, #4058 ) ;
#19791 = CARTESIAN_POINT ( 'NONE',  ( 60.08331549348424971, 8.939227532413909216, 293.5832628385307999 ) ) ;
#19792 = EDGE_LOOP ( 'NONE', ( #12823, #8711, #19133, #4367 ) ) ;
#19793 = DIRECTION ( 'NONE',  ( -0.9396926207859114255, 0.3420201433256601087, -0.000000000000000000 ) ) ;
#19794 = DIRECTION ( 'NONE',  ( 0.2225209339563183342, -0.9749279121818226201, 0.000000000000000000 ) ) ;
#19795 = EDGE_CURVE ( 'NONE', #19254, #3116, #9174, .T. ) ;
#19796 = VERTEX_POINT ( 'NONE', #10454 ) ;
#19797 = LINE ( 'NONE', #5794, #7160 ) ;
#19798 = FACE_OUTER_BOUND ( 'NONE', #12991, .T. ) ;
#19799 = CARTESIAN_POINT ( 'NONE',  ( -130.9868171408399462, -91.88282611735539263, 0.000000000000000000 ) ) ;
#19800 = CYLINDRICAL_SURFACE ( 'NONE', #12439, 15.91767397667355510 ) ;
#19801 = CIRCLE ( 'NONE', #13584, 3.224098631618462552 ) ;
#19802 = CARTESIAN_POINT ( 'NONE',  ( 133.5342034995476297, -80.71481093439410870, 37.85466313993502041 ) ) ;
#19803 = FACE_OUTER_BOUND ( 'NONE', #18389, .T. ) ;
#19804 = ORIENTED_EDGE ( 'NONE', *, *, #11291, .T. ) ;
#19805 = VECTOR ( 'NONE', #18796, 1000.000000000000114 ) ;
#19806 = DIRECTION ( 'NONE',  ( -6.982962677686266711E-15, 0.000000000000000000, -1.000000000000000000 ) ) ;
#19807 = ORIENTED_EDGE ( 'NONE', *, *, #17991, .F. ) ;
#19808 = ORIENTED_EDGE ( 'NONE', *, *, #12902, .F. ) ;
#19809 = CARTESIAN_POINT ( 'NONE',  ( 51.24071425735604635, -32.61983739937743110, 293.5832628385307999 ) ) ;
#19810 = ORIENTED_EDGE ( 'NONE', *, *, #10467, .F. ) ;
#19811 = ORIENTED_EDGE ( 'NONE', *, *, #13333, .T. ) ;
#19812 = CYLINDRICAL_SURFACE ( 'NONE', #4520, 7.500000000000000000 ) ;
#19813 = VECTOR ( 'NONE', #15780, 1000.000000000000114 ) ;
#19814 = CARTESIAN_POINT ( 'NONE',  ( 14.94814811854963210, -76.83212392882498420, 132.4711112102474146 ) ) ;
#19815 = CARTESIAN_POINT ( 'NONE',  ( -48.17797692984161984, -36.99387960884178028, 283.5832628385307999 ) ) ;
#19816 = ORIENTED_EDGE ( 'NONE', *, *, #9024, .T. ) ;
#19817 = CARTESIAN_POINT ( 'NONE',  ( 56.50138340076688337, -22.29928840491054132, 293.5832628385307999 ) ) ;
#19818 = DIRECTION ( 'NONE',  ( -0.000000000000000000, -0.000000000000000000, -1.000000000000000000 ) ) ;
#19819 = VERTEX_POINT ( 'NONE', #8539 ) ;
#19820 = AXIS2_PLACEMENT_3D ( 'NONE', #6264, #15872, #11359 ) ;
#19821 = LINE ( 'NONE', #8579, #4812 ) ;
#19822 = CYLINDRICAL_SURFACE ( 'NONE', #9754, 62.91752772691707207 ) ;
#19823 = CARTESIAN_POINT ( 'NONE',  ( -71.18887634719365565, -147.8252249328922687, 39.99999999999999289 ) ) ;
#19824 = ORIENTED_EDGE ( 'NONE', *, *, #498, .T. ) ;
#19825 = DIRECTION ( 'NONE',  ( 0.000000000000000000, 0.000000000000000000, 1.000000000000000000 ) ) ;
#19826 = CARTESIAN_POINT ( 'NONE',  ( -133.1920331248151399, -82.53376026279585176, 38.51313858039918614 ) ) ;
#19827 = CARTESIAN_POINT ( 'NONE',  ( -100.8303968649779421, 8.087083979452582838, 14.88498244535615633 ) ) ;
#19828 = ORIENTED_EDGE ( 'NONE', *, *, #12850, .F. ) ;
#19829 = FACE_OUTER_BOUND ( 'NONE', #19779, .T. ) ;
#19830 = PLANE ( 'NONE',  #12519 ) ;
#19831 = ORIENTED_EDGE ( 'NONE', *, *, #20235, .T. ) ;
#19832 = ORIENTED_EDGE ( 'NONE', *, *, #9514, .T. ) ;
#19833 = CARTESIAN_POINT ( 'NONE',  ( -97.67167802517903397, -133.7293924297442800, 31.85450751873280240 ) ) ;
#19834 = CIRCLE ( 'NONE', #11020, 112.8770930172170353 ) ;
#19835 = CIRCLE ( 'NONE', #18880, 7.500000000000007105 ) ;
#19836 = ORIENTED_EDGE ( 'NONE', *, *, #15723, .T. ) ;
#19837 = CARTESIAN_POINT ( 'NONE',  ( 51.77251465595239921, -31.77296517111717478, 293.5832628385307999 ) ) ;
#19838 = DIRECTION ( 'NONE',  ( -1.000000000000000000, -0.000000000000000000, -0.000000000000000000 ) ) ;
#19839 = ORIENTED_EDGE ( 'NONE', *, *, #7875, .T. ) ;
#19840 = CARTESIAN_POINT ( 'NONE',  ( 89.41054993672092621, -120.4453604907671718, -5.957062783365469016 ) ) ;
#19841 = DIRECTION ( 'NONE',  ( -0.000000000000000000, -0.000000000000000000, 1.000000000000000000 ) ) ;
#19842 = ADVANCED_FACE ( 'NONE', ( #19678 ), #2500, .F. ) ;
#19843 = EDGE_CURVE ( 'NONE', #16987, #6676, #4283, .T. ) ;
#19844 = AXIS2_PLACEMENT_3D ( 'NONE', #1711, #3452, #4901 ) ;
#19845 = DIRECTION ( 'NONE',  ( -0.000000000000000000, -0.000000000000000000, 1.000000000000000000 ) ) ;
#19846 = PLANE ( 'NONE',  #19642 ) ;
#19847 = CYLINDRICAL_SURFACE ( 'NONE', #13186, 79.75827554147308263 ) ;
#19848 = AXIS2_PLACEMENT_3D ( 'NONE', #15151, #20062, #10845 ) ;
#19849 = PLANE ( 'NONE',  #12162 ) ;
#19850 = CARTESIAN_POINT ( 'NONE',  ( -3.049318610115479988E-17, -0.8794428697894424163, 9.000000000000000000 ) ) ;
#19851 = DIRECTION ( 'NONE',  ( -0.3420201433256757628, 0.9396926207859058744, 0.000000000000000000 ) ) ;
#19852 = DIRECTION ( 'NONE',  ( -1.000000000000000000, 0.000000000000000000, 0.000000000000000000 ) ) ;
#19853 = ORIENTED_EDGE ( 'NONE', *, *, #12390, .T. ) ;
#19854 = EDGE_CURVE ( 'NONE', #14032, #9758, #5934, .T. ) ;
#19855 = CARTESIAN_POINT ( 'NONE',  ( -79.75827554147308263, 9.767571684737763671E-15, 293.5832628385307999 ) ) ;
#19856 = LINE ( 'NONE', #10749, #17087 ) ;
#19857 = EDGE_CURVE ( 'NONE', #3067, #19189, #10535, .T. ) ;
#19858 = ORIENTED_EDGE ( 'NONE', *, *, #10582, .F. ) ;
#19859 = EDGE_CURVE ( 'NONE', #18228, #12122, #11473, .T. ) ;
#19860 = ORIENTED_EDGE ( 'NONE', *, *, #15480, .F. ) ;
#19861 = CIRCLE ( 'NONE', #2239, 42.50000000000000000 ) ;
#19862 = ORIENTED_EDGE ( 'NONE', *, *, #2030, .T. ) ;
#19863 = CARTESIAN_POINT ( 'NONE',  ( 0.000000000000000000, 0.000000000000000000, -100.0000000000000000 ) ) ;
#19864 = ORIENTED_EDGE ( 'NONE', *, *, #4347, .F. ) ;
#19865 = DIRECTION ( 'NONE',  ( -0.000000000000000000, -0.000000000000000000, -1.000000000000000000 ) ) ;
#19866 = CARTESIAN_POINT ( 'NONE',  ( 134.2294018150276145, -76.49442575693798574, 4.443041126027487131 ) ) ;
#19867 = EDGE_CURVE ( 'NONE', #12798, #20089, #17024, .T. ) ;
#19868 = DIRECTION ( 'NONE',  ( -0.000000000000000000, -0.000000000000000000, 1.000000000000000000 ) ) ;
#19869 = DIRECTION ( 'NONE',  ( 0.4338837391175549563, 0.9009688679024205893, 0.000000000000000000 ) ) ;
#19870 = DIRECTION ( 'NONE',  ( 0.000000000000000000, 0.000000000000000000, -1.000000000000000000 ) ) ;
#19871 = EDGE_LOOP ( 'NONE', ( #8881, #13612, #18590, #6916 ) ) ;
#19872 = CARTESIAN_POINT ( 'NONE',  ( -22.29928840491073316, -56.50138340076681231, 283.5832628385307999 ) ) ;
#19873 = CARTESIAN_POINT ( 'NONE',  ( -134.6114153021046320, -66.18050771012671873, 4.130514097776864624 ) ) ;
#19874 = CARTESIAN_POINT ( 'NONE',  ( 129.0008258633897640, -76.61840651136441238, -0.1009346208872797107 ) ) ;
#19875 = AXIS2_PLACEMENT_3D ( 'NONE', #3052, #9068, #10911 ) ;
#19876 = CARTESIAN_POINT ( 'NONE',  ( -166.7850001792984926, -190.0000000000000284, 40.00000000000000000 ) ) ;
#19877 = FACE_OUTER_BOUND ( 'NONE', #8960, .T. ) ;
#19878 = VECTOR ( 'NONE', #4021, 1000.000000000000000 ) ;
#19879 = CARTESIAN_POINT ( 'NONE',  ( 97.50000000000002842, -195.8578643762690206, 35.85786437626904188 ) ) ;
#19880 = AXIS2_PLACEMENT_3D ( 'NONE', #19138, #13077, #16469 ) ;
#19881 = ORIENTED_EDGE ( 'NONE', *, *, #7661, .F. ) ;
#19882 = AXIS2_PLACEMENT_3D ( 'NONE', #4349, #10577, #1287 ) ;
#19883 = LINE ( 'NONE', #4235, #10196 ) ;
#19884 = EDGE_CURVE ( 'NONE', #8089, #2316, #15485, .T. ) ;
#19885 = EDGE_CURVE ( 'NONE', #7332, #1702, #2907, .T. ) ;
#19886 = ORIENTED_EDGE ( 'NONE', *, *, #12870, .T. ) ;
#19887 = EDGE_CURVE ( 'NONE', #6652, #6960, #13735, .T. ) ;
#19888 = ORIENTED_EDGE ( 'NONE', *, *, #19156, .F. ) ;
#19889 = ORIENTED_EDGE ( 'NONE', *, *, #7749, .T. ) ;
#19890 = ORIENTED_EDGE ( 'NONE', *, *, #11146, .F. ) ;
#19891 = AXIS2_PLACEMENT_3D ( 'NONE', #12861, #13149, #5300 ) ;
#19892 = VECTOR ( 'NONE', #1819, 1000.000000000000000 ) ;
#19893 = EDGE_CURVE ( 'NONE', #2847, #4825, #3944, .T. ) ;
#19894 = DIRECTION ( 'NONE',  ( 0.000000000000000000, -0.5000000000000013323, -0.8660254037844380415 ) ) ;
#19895 = LINE ( 'NONE', #19791, #13651 ) ;
#19896 = ORIENTED_EDGE ( 'NONE', *, *, #11164, .F. ) ;
#19897 = CARTESIAN_POINT ( 'NONE',  ( -167.4599531637108782, -36.50981547337168109, 49.99999999999999289 ) ) ;
#19898 = DIRECTION ( 'NONE',  ( 1.000000000000000000, 0.000000000000000000, 0.000000000000000000 ) ) ;
#19899 = ORIENTED_EDGE ( 'NONE', *, *, #3384, .T. ) ;
#19900 = CARTESIAN_POINT ( 'NONE',  ( -108.6450314030896891, 75.64087399529431366, -29.99999999999949196 ) ) ;
#19901 = DIRECTION ( 'NONE',  ( 0.6155349844899687950, -0.7881095627315619634, 0.000000000000000000 ) ) ;
#19902 = LINE ( 'NONE', #13549, #18591 ) ;
#19903 = DIRECTION ( 'NONE',  ( 1.000000000000000000, 0.000000000000000000, 0.000000000000000000 ) ) ;
#19904 = EDGE_CURVE ( 'NONE', #13184, #13146, #5877, .T. ) ;
#19905 = CARTESIAN_POINT ( 'NONE',  ( 132.2990932590224702, -86.73761849286395886, 39.55987232456632086 ) ) ;
#19906 = CARTESIAN_POINT ( 'NONE',  ( 144.1130761623740568, -69.50842595698583182, 49.99999999999999289 ) ) ;
#19907 = CIRCLE ( 'NONE', #19573, 15.91767397667354444 ) ;
#19908 = EDGE_LOOP ( 'NONE', ( #8020, #883, #11161, #638 ) ) ;
#19909 = CARTESIAN_POINT ( 'NONE',  ( -176.5810126522742394, -187.6736222527391647, 31.17213215707407414 ) ) ;
#19910 = ORIENTED_EDGE ( 'NONE', *, *, #5991, .F. ) ;
#19911 = ADVANCED_FACE ( 'NONE', ( #9243 ), #7396, .T. ) ;
#19912 = ORIENTED_EDGE ( 'NONE', *, *, #7890, .F. ) ;
#19913 = LINE ( 'NONE', #18287, #18734 ) ;
#19914 = EDGE_LOOP ( 'NONE', ( #18846, #10755, #1995, #2732 ) ) ;
#19915 = DIRECTION ( 'NONE',  ( -0.2225209339563195554, 0.9749279121818223981, 0.000000000000000000 ) ) ;
#19916 = LINE ( 'NONE', #4369, #10083 ) ;
#19917 = CARTESIAN_POINT ( 'NONE',  ( 123.8492616149702741, -72.31991210363503342, 10.00000000000000178 ) ) ;
#19918 = FACE_OUTER_BOUND ( 'NONE', #15731, .T. ) ;
#19919 = ORIENTED_EDGE ( 'NONE', *, *, #9270, .F. ) ;
#19920 = AXIS2_PLACEMENT_3D ( 'NONE', #15481, #1152, #7393 ) ;
#19921 = DIRECTION ( 'NONE',  ( -0.000000000000000000, -0.000000000000000000, 1.000000000000000000 ) ) ;
#19922 = CARTESIAN_POINT ( 'NONE',  ( 54.07248341783254375, -32.16802499836760632, 132.4711112102474146 ) ) ;
#19923 = ORIENTED_EDGE ( 'NONE', *, *, #11106, .F. ) ;
#19924 = CARTESIAN_POINT ( 'NONE',  ( 0.000000000000000000, 164.0736214083062805, 60.00000000000000000 ) ) ;
#19925 = PLANE ( 'NONE',  #4198 ) ;
#19926 = DIRECTION ( 'NONE',  ( 6.982962677686266711E-15, -0.000000000000000000, 1.000000000000000000 ) ) ;
#19927 = ORIENTED_EDGE ( 'NONE', *, *, #2474, .F. ) ;
#19928 = FACE_OUTER_BOUND ( 'NONE', #2748, .T. ) ;
#19929 = CARTESIAN_POINT ( 'NONE',  ( -134.6261364156839591, -73.66016459667358163, 32.57698633332318394 ) ) ;
#19930 = DIRECTION ( 'NONE',  ( -4.650550193362991910E-16, -1.000000000000000000, 0.000000000000000000 ) ) ;
#19931 = ORIENTED_EDGE ( 'NONE', *, *, #10405, .T. ) ;
#19932 = VECTOR ( 'NONE', #16375, 1000.000000000000000 ) ;
#19933 = FACE_BOUND ( 'NONE', #7019, .T. ) ;
#19934 = DIRECTION ( 'NONE',  ( -6.982962677686266711E-15, 0.000000000000000000, -1.000000000000000000 ) ) ;
#19935 = PRODUCT_DEFINITION_FORMATION_WITH_SPECIFIED_SOURCE ( 'ANY', '', #14221, .NOT_KNOWN. ) ;
#19936 = ORIENTED_EDGE ( 'NONE', *, *, #14984, .T. ) ;
#19937 = VECTOR ( 'NONE', #11072, 1000.000000000000114 ) ;
#19938 = EDGE_LOOP ( 'NONE', ( #9893, #15201, #13535, #12586, #190, #7086, #7058, #11271, #8039 ) ) ;
#19939 = CARTESIAN_POINT ( 'NONE',  ( -28.06281046684226155, 73.06915264522029929, 111.4180192758973931 ) ) ;
#19940 = ORIENTED_EDGE ( 'NONE', *, *, #987, .F. ) ;
#19941 = CARTESIAN_POINT ( 'NONE',  ( -3.911853314815648908, 4.196299268919088554, 293.5832628385307999 ) ) ;
#19942 = PLANE ( 'NONE',  #1747 ) ;
#19943 = EDGE_LOOP ( 'NONE', ( #17989, #14263, #7095, #11313 ) ) ;
#19944 = CARTESIAN_POINT ( 'NONE',  ( 83.97601510867102093, -124.2902204837746893, 1.122958062864681583 ) ) ;
#19945 = CARTESIAN_POINT ( 'NONE',  ( 0.000000000000000000, 17.50000000000001066, 83.57543755549745867 ) ) ;
#19946 = VECTOR ( 'NONE', #19698, 1000.000000000000114 ) ;
#19947 = VECTOR ( 'NONE', #6759, 1000.000000000000114 ) ;
#19948 = DIRECTION ( 'NONE',  ( 0.000000000000000000, 0.000000000000000000, 1.000000000000000000 ) ) ;
#19949 = CARTESIAN_POINT ( 'NONE',  ( 0.000000000000000000, 0.000000000000000000, 293.5832628385307999 ) ) ;
#19950 = CARTESIAN_POINT ( 'NONE',  ( -97.95177330934008353, 59.60912842347561025, 39.88498244535613679 ) ) ;
#19951 = CARTESIAN_POINT ( 'NONE',  ( -14.02132266220276691, 20.55229278271246329, 14.88498244535555060 ) ) ;
#19952 = DIRECTION ( 'NONE',  ( -1.000000000000000000, 0.000000000000000000, 0.000000000000000000 ) ) ;
#19953 = CARTESIAN_POINT ( 'NONE',  ( 82.03125000078792084, -125.5821405427867461, 31.51013335451832731 ) ) ;
#19954 = ORIENTED_EDGE ( 'NONE', *, *, #10775, .F. ) ;
#19955 = DIRECTION ( 'NONE',  ( 1.000000000000000000, 0.000000000000000000, 0.000000000000000000 ) ) ;
#19956 = CARTESIAN_POINT ( 'NONE',  ( -61.70726652483826058, -12.28122767885825084, 293.5832628385307999 ) ) ;
#19957 = EDGE_LOOP ( 'NONE', ( #1411, #14639, #10829, #13194 ) ) ;
#19958 = EDGE_CURVE ( 'NONE', #4164, #12652, #3113, .T. ) ;
#19959 = AXIS2_PLACEMENT_3D ( 'NONE', #16069, #9918, #16169 ) ;
#19960 = ORIENTED_EDGE ( 'NONE', *, *, #14166, .F. ) ;
#19961 =( LENGTH_UNIT ( ) NAMED_UNIT ( * ) SI_UNIT ( .MILLI., .METRE. ) );
#19962 = VECTOR ( 'NONE', #18350, 1000.000000000000000 ) ;
#19963 = ORIENTED_EDGE ( 'NONE', *, *, #14156, .T. ) ;
#19964 = FACE_BOUND ( 'NONE', #16531, .T. ) ;
#19965 = ORIENTED_EDGE ( 'NONE', *, *, #18772, .F. ) ;
#19966 = DIRECTION ( 'NONE',  ( 0.000000000000000000, 0.000000000000000000, 1.000000000000000000 ) ) ;
#19967 = CARTESIAN_POINT ( 'NONE',  ( 28.63313560863472063, -51.23821591265105013, 132.4711112102474146 ) ) ;
#19968 = DIRECTION ( 'NONE',  ( 0.000000000000000000, 1.000000000000000000, 0.000000000000000000 ) ) ;
#19969 = EDGE_CURVE ( 'NONE', #3588, #9534, #6291, .T. ) ;
#19970 = CARTESIAN_POINT ( 'NONE',  ( 86.01343624116272224, 31.38211805825951473, 40.00000000000000000 ) ) ;
#19971 = ADVANCED_FACE ( 'NONE', ( #4327 ), #10664, .T. ) ;
#19972 = DIRECTION ( 'NONE',  ( -0.1736481776669207000, -0.9848077530122097967, 0.000000000000000000 ) ) ;
#19973 = CYLINDRICAL_SURFACE ( 'NONE', #18928, 17.50000000000001066 ) ;
#19974 = ORIENTED_EDGE ( 'NONE', *, *, #601, .F. ) ;
#19975 = EDGE_CURVE ( 'NONE', #6026, #18385, #5978, .T. ) ;
#19976 = FACE_OUTER_BOUND ( 'NONE', #19655, .T. ) ;
#19977 = CARTESIAN_POINT ( 'NONE',  ( 144.1955966362266679, 102.2982297021113141, 49.99999999999999289 ) ) ;
#19978 = CARTESIAN_POINT ( 'NONE',  ( 130.9519479124748784, -73.15688856708820254, -5.283951177996526027 ) ) ;
#19979 = DIRECTION ( 'NONE',  ( -0.4999999999999950040, -0.8660254037844415942, 0.000000000000000000 ) ) ;
#19980 = DIRECTION ( 'NONE',  ( 0.000000000000000000, -0.4999999999999998335, 0.8660254037844387076 ) ) ;
#19981 = VERTEX_POINT ( 'NONE', #18668 ) ;
#19982 = FACE_OUTER_BOUND ( 'NONE', #16796, .T. ) ;
#19983 = EDGE_CURVE ( 'NONE', #4216, #19621, #16815, .T. ) ;
#19984 = ORIENTED_EDGE ( 'NONE', *, *, #6874, .T. ) ;
#19985 = ORIENTED_EDGE ( 'NONE', *, *, #17241, .T. ) ;
#19986 = ORIENTED_EDGE ( 'NONE', *, *, #16637, .T. ) ;
#19987 = CARTESIAN_POINT ( 'NONE',  ( 106.5208805777952676, 53.25886146954521649, 14.88498244535470683 ) ) ;
#19988 = EDGE_CURVE ( 'NONE', #18469, #1901, #1574, .T. ) ;
#19989 = AXIS2_PLACEMENT_3D ( 'NONE', #1989, #8216, #16205 ) ;
#19990 = FACE_OUTER_BOUND ( 'NONE', #19938, .T. ) ;
#19991 = EDGE_LOOP ( 'NONE', ( #20049, #11098, #13882, #15719 ) ) ;
#19992 = VECTOR ( 'NONE', #256, 1000.000000000000000 ) ;
#19993 = EDGE_CURVE ( 'NONE', #13679, #6744, #16390, .T. ) ;
#19994 = CARTESIAN_POINT ( 'NONE',  ( -7.499999999999583444, -60.00000000000000000, -115.0000000000000000 ) ) ;
#19995 = DIRECTION ( 'NONE',  ( -0.03505990758545545621, -0.9993852124581888985, 0.000000000000000000 ) ) ;
#19996 = EDGE_CURVE ( 'NONE', #12285, #1203, #1335, .T. ) ;
#19997 = ORIENTED_EDGE ( 'NONE', *, *, #11265, .T. ) ;
#19998 = CYLINDRICAL_SURFACE ( 'NONE', #19882, 62.91752772691707207 ) ;
#19999 = CARTESIAN_POINT ( 'NONE',  ( 60.00000000000000711, 6.284666409917639535E-13, -100.0000000000000000 ) ) ;
#20000 = LINE ( 'NONE', #2429, #14346 ) ;
#20001 = AXIS2_PLACEMENT_3D ( 'NONE', #8788, #10130, #16279 ) ;
#20002 = LINE ( 'NONE', #12223, #17028 ) ;
#20003 = AXIS2_PLACEMENT_3D ( 'NONE', #18222, #8902, #15456 ) ;
#20004 = CARTESIAN_POINT ( 'NONE',  ( -29.99999999999887379, 275.0000000000000000, 4.999999999999158007 ) ) ;
#20005 = CARTESIAN_POINT ( 'NONE',  ( -17.49999999999999289, 0.000000000000000000, 49.99999999999999289 ) ) ;
#20006 = ORIENTED_EDGE ( 'NONE', *, *, #12516, .F. ) ;
#20007 = ORIENTED_EDGE ( 'NONE', *, *, #14234, .F. ) ;
#20008 = EDGE_CURVE ( 'NONE', #8838, #16933, #14417, .T. ) ;
#20009 = DIRECTION ( 'NONE',  ( -4.650550193362991910E-16, -1.000000000000000000, 0.000000000000000000 ) ) ;
#20010 = AXIS2_PLACEMENT_3D ( 'NONE', #2359, #4082, #19346 ) ;
#20011 = VECTOR ( 'NONE', #20057, 1000.000000000000000 ) ;
#20012 = ORIENTED_EDGE ( 'NONE', *, *, #9416, .F. ) ;
#20013 = ORIENTED_EDGE ( 'NONE', *, *, #4154, .F. ) ;
#20014 = CARTESIAN_POINT ( 'NONE',  ( -73.25972925305609351, 27.53920554013712874, 111.4180192758973931 ) ) ;
#20015 = ORIENTED_EDGE ( 'NONE', *, *, #16413, .F. ) ;
#20016 = EDGE_LOOP ( 'NONE', ( #18957, #12328, #8620 ) ) ;
#20017 = AXIS2_PLACEMENT_3D ( 'NONE', #5507, #11729, #14905 ) ;
#20018 = FACE_OUTER_BOUND ( 'NONE', #18999, .T. ) ;
#20019 = CYLINDRICAL_SURFACE ( 'NONE', #5677, 60.74260934110282051 ) ;
#20020 = DIRECTION ( 'NONE',  ( -0.000000000000000000, -0.000000000000000000, -1.000000000000000000 ) ) ;
#20021 = ORIENTED_EDGE ( 'NONE', *, *, #4288, .F. ) ;
#20022 = EDGE_CURVE ( 'NONE', #15118, #17837, #17127, .T. ) ;
#20023 = ADVANCED_FACE ( 'NONE', ( #7499 ), #12301, .F. ) ;
#20024 = DIRECTION ( 'NONE',  ( -0.000000000000000000, -1.000000000000000000, -0.000000000000000000 ) ) ;
#20025 = LINE ( 'NONE', #4904, #17306 ) ;
#20026 = ADVANCED_FACE ( 'NONE', ( #18870 ), #12813, .F. ) ;
#20027 = ORIENTED_EDGE ( 'NONE', *, *, #8274, .F. ) ;
#20028 = EDGE_CURVE ( 'NONE', #12028, #6717, #2007, .T. ) ;
#20029 = CARTESIAN_POINT ( 'NONE',  ( -77.12898346057446020, 127.7594922753211080, -17.80027040494307400 ) ) ;
#20031 = AXIS2_PLACEMENT_3D ( 'NONE', #13896, #16870, #12255 ) ;
#20030 = LINE ( 'NONE', #7443, #5841 ) ;
#20032 = CIRCLE ( 'NONE', #1736, 7.500000000000006217 ) ;
#20033 = LINE ( 'NONE', #18404, #5399 ) ;
#20034 = DIRECTION ( 'NONE',  ( 0.000000000000000000, 1.000000000000000000, 0.000000000000000000 ) ) ;
#20035 = VECTOR ( 'NONE', #1251, 999.9999999999998863 ) ;
#20036 = CARTESIAN_POINT ( 'NONE',  ( -134.2873401242900968, -76.10409495552310943, 35.26608652156301815 ) ) ;
#20037 = CARTESIAN_POINT ( 'NONE',  ( -101.1986828041967499, 96.79850148450320546, 38.95247587951536872 ) ) ;
#20038 = ORIENTED_EDGE ( 'NONE', *, *, #12976, .T. ) ;
#20039 = DIRECTION ( 'NONE',  ( -0.000000000000000000, -0.000000000000000000, -1.000000000000000000 ) ) ;
#20040 = FACE_OUTER_BOUND ( 'NONE', #9350, .T. ) ;
#20041 = ORIENTED_EDGE ( 'NONE', *, *, #7977, .F. ) ;
#20042 =( REPRESENTATION_RELATIONSHIP ('NONE','NONE', #17382, #15821 ) REPRESENTATION_RELATIONSHIP_WITH_TRANSFORMATION ( #3792 )SHAPE_REPRESENTATION_RELATIONSHIP( ) );
#20043 = EDGE_LOOP ( 'NONE', ( #11683, #6943, #1385, #3911 ) ) ;
#20044 = CARTESIAN_POINT ( 'NONE',  ( -82.03124999999998579, -125.5821405433014348, 30.00000000000001776 ) ) ;
#20045 = VECTOR ( 'NONE', #3760, 1000.000000000000000 ) ;
#20046 = EDGE_LOOP ( 'NONE', ( #13107, #8509 ) ) ;
#20047 = CARTESIAN_POINT ( 'NONE',  ( -113.9638382236393710, 83.66658905436058546, -34.85447305243185667 ) ) ;
#20048 = DIRECTION ( 'NONE',  ( -0.000000000000000000, -0.000000000000000000, -1.000000000000000000 ) ) ;
#20049 = ORIENTED_EDGE ( 'NONE', *, *, #2417, .F. ) ;
#20050 = CIRCLE ( 'NONE', #6998, 112.8770930172170068 ) ;
#20051 = CARTESIAN_POINT ( 'NONE',  ( 98.61806909068849336, -132.4668554876670896, 5.401815755557273668 ) ) ;
#20052 = CARTESIAN_POINT ( 'NONE',  ( 0.000000000000000000, 0.000000000000000000, 283.5832628385307999 ) ) ;
#20053 = ADVANCED_FACE ( 'NONE', ( #3617 ), #12608, .T. ) ;
#20054 = CARTESIAN_POINT ( 'NONE',  ( -138.0190094366552387, -24.44405370507808328, -10.87470759034249745 ) ) ;
#20055 = DIRECTION ( 'NONE',  ( -0.3420201433256757073, 0.9396926207859057634, 0.000000000000000000 ) ) ;
#20056 = LINE ( 'NONE', #16993, #11581 ) ;
#20057 = DIRECTION ( 'NONE',  ( 0.000000000000000000, 0.000000000000000000, -1.000000000000000000 ) ) ;
#20058 = DIRECTION ( 'NONE',  ( 0.000000000000000000, 0.000000000000000000, -1.000000000000000000 ) ) ;
#20059 = CARTESIAN_POINT ( 'NONE',  ( -60.00000000000000000, -2.094888803305880013E-13, -115.0000000000000000 ) ) ;
#20060 = CARTESIAN_POINT ( 'NONE',  ( 95.49560220035800739, -115.9193184531417131, 33.43809937674511445 ) ) ;
#20061 = ORIENTED_EDGE ( 'NONE', *, *, #12135, .T. ) ;
#20062 = DIRECTION ( 'NONE',  ( 0.000000000000000000, 1.000000000000000000, -0.000000000000000000 ) ) ;
#20063 = LINE ( 'NONE', #19956, #10869 ) ;
#20064 = ORIENTED_EDGE ( 'NONE', *, *, #5007, .T. ) ;
#20065 = AXIS2_PLACEMENT_3D ( 'NONE', #14224, #17611, #3386 ) ;
#20066 = VERTEX_POINT ( 'NONE', #9845 ) ;
#20067 = VECTOR ( 'NONE', #9465, 1000.000000000000000 ) ;
#20068 = ORIENTED_EDGE ( 'NONE', *, *, #19033, .T. ) ;
#20069 = DIRECTION ( 'NONE',  ( -0.000000000000000000, -0.000000000000000000, -1.000000000000000000 ) ) ;
#20070 = ORIENTED_EDGE ( 'NONE', *, *, #15010, .F. ) ;
#20071 = CARTESIAN_POINT ( 'NONE',  ( -39.37628763770455009, -49.07263256785938665, 132.4711112102474146 ) ) ;
#20072 = CARTESIAN_POINT ( 'NONE',  ( 56.84754764479240663, -154.7316448359447634, 39.99999999999999289 ) ) ;
#20073 = DIRECTION ( 'NONE',  ( 0.5060387318153625191, 6.197187131622696351E-17, -0.8625107546591518348 ) ) ;
#20074 = LINE ( 'NONE', #19970, #7464 ) ;
#20075 = AXIS2_PLACEMENT_3D ( 'NONE', #5520, #17808, #3778 ) ;
#20076 = FACE_OUTER_BOUND ( 'NONE', #13190, .T. ) ;
#20077 = CARTESIAN_POINT ( 'NONE',  ( 0.000000000000000000, 0.000000000000000000, 248.9926560891072143 ) ) ;
#20078 = ADVANCED_FACE ( 'NONE', ( #14456 ), #17444, .T. ) ;
#20079 = CARTESIAN_POINT ( 'NONE',  ( -20.21777810286715749, -59.58067424803620327, 132.4711112102474146 ) ) ;
#20080 = CARTESIAN_POINT ( 'NONE',  ( -134.0645693066666411, -77.56608579646530188, 3.731507865007667846 ) ) ;
#20081 = CARTESIAN_POINT ( 'NONE',  ( 130.5436973595105030, -73.98181611796424306, 1.254900387872837531 ) ) ;
#20082 = DIRECTION ( 'NONE',  ( 0.000000000000000000, 0.000000000000000000, 1.000000000000000000 ) ) ;
#20083 = CARTESIAN_POINT ( 'NONE',  ( 126.5370453525553955, 80.55045718954892209, 49.99999999999999289 ) ) ;
#20084 = CARTESIAN_POINT ( 'NONE',  ( -132.3196846491782424, -70.65764850136368125, 43.06549271861968720 ) ) ;
#20085 = VERTEX_POINT ( 'NONE', #138 ) ;
#20086 = PLANE ( 'NONE',  #18714 ) ;
#20087 = AXIS2_PLACEMENT_3D ( 'NONE', #17506, #17900, #8279 ) ;
#20088 = ADVANCED_FACE ( 'NONE', ( #9647 ), #238, .F. ) ;
#20089 = VERTEX_POINT ( 'NONE', #446 ) ;
#20090 = CIRCLE ( 'NONE', #6057, 62.91752772691707207 ) ;
#20091 = ORIENTED_EDGE ( 'NONE', *, *, #8638, .F. ) ;
#20092 = ORIENTED_EDGE ( 'NONE', *, *, #14262, .F. ) ;
#20093 = CARTESIAN_POINT ( 'NONE',  ( -9.564549117045517690, -62.18629025319811632, 132.4711112102474146 ) ) ;
#20094 = LINE ( 'NONE', #15080, #8634 ) ;
#20095 = FACE_OUTER_BOUND ( 'NONE', #5790, .T. ) ;
#20096 = ORIENTED_EDGE ( 'NONE', *, *, #8554, .F. ) ;
#20098 = DIRECTION ( 'NONE',  ( -0.000000000000000000, 0.000000000000000000, -1.000000000000000000 ) ) ;
#20097 = AXIS2_PLACEMENT_3D ( 'NONE', #13908, #6151, #7770 ) ;
#20099 = CYLINDRICAL_SURFACE ( 'NONE', #16330, 106.4288957539800862 ) ;
#20100 = EDGE_CURVE ( 'NONE', #12873, #625, #18675, .T. ) ;
#20101 = EDGE_LOOP ( 'NONE', ( #15703, #8350, #8153, #6351, #19214, #5309 ) ) ;
#20102 = DIRECTION ( 'NONE',  ( -1.000000000000000000, -0.000000000000000000, -0.000000000000000000 ) ) ;
#20103 = FACE_OUTER_BOUND ( 'NONE', #15389, .T. ) ;
#20104 = DIRECTION ( 'NONE',  ( -1.000000000000000000, 0.000000000000000000, 0.000000000000000000 ) ) ;
#20105 = DIRECTION ( 'NONE',  ( 0.000000000000000000, -1.000000000000000000, 0.000000000000000000 ) ) ;
#20106 = FACE_OUTER_BOUND ( 'NONE', #14514, .T. ) ;
#20107 = CARTESIAN_POINT ( 'NONE',  ( 132.9648440817097708, -83.65857578542980377, 38.84409438298517614 ) ) ;
#20108 = CARTESIAN_POINT ( 'NONE',  ( 37.78325588002174840, -47.56406379474564972, 293.5832628385307999 ) ) ;
#20109 = ORIENTED_EDGE ( 'NONE', *, *, #18159, .T. ) ;
#20110 = EDGE_LOOP ( 'NONE', ( #7283, #2484, #12578, #10269 ) ) ;
#20111 = ADVANCED_FACE ( 'NONE', ( #15896 ), #16376, .T. ) ;
#20112 = VERTEX_POINT ( 'NONE', #8009 ) ;
#20113 = AXIS2_PLACEMENT_3D ( 'NONE', #10498, #15316, #16752 ) ;
#20114 = VERTEX_POINT ( 'NONE', #6592 ) ;
#20115 = EDGE_CURVE ( 'NONE', #1303, #9432, #337, .T. ) ;
#20116 = DIRECTION ( 'NONE',  ( 0.000000000000000000, 0.000000000000000000, -1.000000000000000000 ) ) ;
#20117 = EDGE_LOOP ( 'NONE', ( #14875, #1668 ) ) ;
#20118 = VERTEX_POINT ( 'NONE', #17340 ) ;
#20119 = DIRECTION ( 'NONE',  ( 1.000000000000000000, 0.000000000000000000, -0.000000000000000000 ) ) ;
#20120 = CARTESIAN_POINT ( 'NONE',  ( 19.30071112029679625, -55.43188410062176530, 248.9926560891072143 ) ) ;
#20121 = DIRECTION ( 'NONE',  ( 0.000000000000000000, 0.000000000000000000, 1.000000000000000000 ) ) ;
#20122 = EDGE_LOOP ( 'NONE', ( #18080, #5089, #5610, #5442 ) ) ;
#20123 = DIRECTION ( 'NONE',  ( 1.000000000000000000, 0.000000000000000000, 0.000000000000000000 ) ) ;
#20124 = CARTESIAN_POINT ( 'NONE',  ( -76.92888220842476699, 14.39940464655785313, 132.4711112102474146 ) ) ;
#20125 = CIRCLE ( 'NONE', #11312, 15.91767397667355510 ) ;
#20126 = EDGE_LOOP ( 'NONE', ( #11466, #12244, #18360, #16662 ) ) ;
#20127 = CIRCLE ( 'NONE', #10654, 99.99999999999997158 ) ;
#20128 = ADVANCED_FACE ( 'NONE', ( #17542 ), #8312, .T. ) ;
#20129 = CARTESIAN_POINT ( 'NONE',  ( 0.000000000000000000, 0.000000000000000000, -100.0000000000000000 ) ) ;
#20130 = CARTESIAN_POINT ( 'NONE',  ( 53.87178215532755132, 28.06680738835045119, 283.5832628385307999 ) ) ;
#20131 = CARTESIAN_POINT ( 'NONE',  ( 7.948651060879040386, -60.22029172860440127, 293.5832628385307999 ) ) ;
#20132 = VECTOR ( 'NONE', #18379, 1000.000000000000000 ) ;
#20133 = DIRECTION ( 'NONE',  ( 1.000000000000000000, 0.000000000000000000, -6.994638739193269649E-15 ) ) ;
#20134 = FACE_OUTER_BOUND ( 'NONE', #3791, .T. ) ;
#20135 = CARTESIAN_POINT ( 'NONE',  ( -82.10917641232227027, 113.4001070177828154, 26.20091274746184240 ) ) ;
#20136 = ORIENTED_EDGE ( 'NONE', *, *, #2673, .T. ) ;
#20137 = LINE ( 'NONE', #12254, #12336 ) ;
#20138 = CARTESIAN_POINT ( 'NONE',  ( 0.000000000000000000, 79.75827554147308263, 132.4711112102474146 ) ) ;
#20139 = EDGE_LOOP ( 'NONE', ( #11423, #3091, #7530, #16457 ) ) ;
#20140 = ADVANCED_FACE ( 'NONE', ( #12712 ), #6793, .T. ) ;
#20142 = EDGE_CURVE ( 'NONE', #10253, #3366, #12739, .T. ) ;
#20141 = AXIS2_PLACEMENT_3D ( 'NONE', #5299, #3659, #11123 ) ;
#20143 = ORIENTED_EDGE ( 'NONE', *, *, #6760, .T. ) ;
#20144 = EDGE_CURVE ( 'NONE', #12002, #937, #15998, .T. ) ;
#20145 = PRODUCT_RELATED_PRODUCT_CATEGORY ( 'part', '', ( #3622 ) ) ;
#20146 = CARTESIAN_POINT ( 'NONE',  ( -96.67521566530153621, -115.8170149451950692, 29.68188518566230982 ) ) ;
#20147 = AXIS2_PLACEMENT_3D ( 'NONE', #19545, #6876, #920 ) ;
#20148 = ORIENTED_EDGE ( 'NONE', *, *, #5394, .F. ) ;
#20149 = CARTESIAN_POINT ( 'NONE',  ( -136.3855242278113735, 54.99785135045119944, -25.06786605331940621 ) ) ;
#20150 = DIRECTION ( 'NONE',  ( 0.000000000000000000, 0.000000000000000000, 1.000000000000000000 ) ) ;
#20151 = ORIENTED_EDGE ( 'NONE', *, *, #8839, .F. ) ;
#20152 = CARTESIAN_POINT ( 'NONE',  ( 99.35210738963728261, -131.4612102079554177, 4.192299627536158368 ) ) ;
#20153 = CARTESIAN_POINT ( 'NONE',  ( 62.91215678473958661, -0.8220851292428736912, 132.4711112102474146 ) ) ;
#20154 = ADVANCED_FACE ( 'NONE', ( #1985 ), #5256, .F. ) ;
#20155 = ADVANCED_FACE ( 'NONE', ( #7905 ), #14152, .F. ) ;
#20156 = DIRECTION ( 'NONE',  ( -0.000000000000000000, -1.000000000000000000, -0.000000000000000000 ) ) ;
#20157 =( LENGTH_UNIT ( ) NAMED_UNIT ( * ) SI_UNIT ( .MILLI., .METRE. ) );
#20158 = VERTEX_POINT ( 'NONE', #8708 ) ;
#20159 = PLANE ( 'NONE',  #9221 ) ;
#20160 = CARTESIAN_POINT ( 'NONE',  ( 0.07568653364411945250, -1.751902528157375905, 8.999999999999996447 ) ) ;
#20161 = PLANE ( 'NONE',  #12154 ) ;
#20162 = CARTESIAN_POINT ( 'NONE',  ( 82.03125000000002842, -125.5821405433014064, 30.00000000000000000 ) ) ;
#20163 = ORIENTED_EDGE ( 'NONE', *, *, #1389, .F. ) ;
#20164 = VECTOR ( 'NONE', #11228, 1000.000000000000114 ) ;
#20165 = DIRECTION ( 'NONE',  ( 0.000000000000000000, 0.000000000000000000, 1.000000000000000000 ) ) ;
#20166 = DIRECTION ( 'NONE',  ( -0.6427876096865353661, -0.7660444431189813441, -0.000000000000000000 ) ) ;
#20167 = EDGE_CURVE ( 'NONE', #19300, #858, #11582, .T. ) ;
#20168 = ORIENTED_EDGE ( 'NONE', *, *, #6018, .T. ) ;
#20169 = VERTEX_POINT ( 'NONE', #3906 ) ;
#20170 = PRODUCT_CONTEXT ( 'NONE', #15871, 'mechanical' ) ;
#20171 = ORIENTED_EDGE ( 'NONE', *, *, #10775, .T. ) ;
#20172 = EDGE_CURVE ( 'NONE', #4825, #15881, #4000, .T. ) ;
#20173 = CARTESIAN_POINT ( 'NONE',  ( -103.4088548222096620, -125.4447869035480210, 0.8709733734652972403 ) ) ;
#20174 = LINE ( 'NONE', #9440, #4457 ) ;
#20175 = EDGE_LOOP ( 'NONE', ( #4213, #1283, #11699, #6501 ) ) ;
#20176 = LINE ( 'NONE', #9333, #2074 ) ;
#20177 = CARTESIAN_POINT ( 'NONE',  ( 62.91752772691707207, 0.000000000000000000, 83.57543755549745867 ) ) ;
#20178 = CARTESIAN_POINT ( 'NONE',  ( -97.49999999999997158, -115.4778303846450029, 10.00000000000000355 ) ) ;
#20179 = CIRCLE ( 'NONE', #5808, 60.74260934110282051 ) ;
#20180 = AXIS2_PLACEMENT_3D ( 'NONE', #19510, #6738, #9998 ) ;
#20181 = CARTESIAN_POINT ( 'NONE',  ( -96.21889527877688408, -115.1753595937449575, 35.54861044090515776 ) ) ;
#20182 = CARTESIAN_POINT ( 'NONE',  ( 37.78325588002174840, -47.56406379474564972, 293.5832628385307999 ) ) ;
#20183 = CARTESIAN_POINT ( 'NONE',  ( 0.000000000000000000, 0.000000000000000000, 293.5832628385307999 ) ) ;
#20184 = CARTESIAN_POINT ( 'NONE',  ( 47.66508197439472383, -41.06890862491489003, 248.9926560891072143 ) ) ;
#20185 = DIRECTION ( 'NONE',  ( -0.000000000000000000, -0.000000000000000000, -1.000000000000000000 ) ) ;
#20186 = CARTESIAN_POINT ( 'NONE',  ( 125.0010599886705620, -82.93257931482615675, -0.9426074830654761483 ) ) ;
#20187 = DIRECTION ( 'NONE',  ( 0.8660254037844432595, -0.4999999999999919509, 0.000000000000000000 ) ) ;
#20188 = LINE ( 'NONE', #8930, #14620 ) ;
#20189 = CARTESIAN_POINT ( 'NONE',  ( -131.8276101104381439, -71.67687255337297358, 36.69851420954442744 ) ) ;
#20190 = ORIENTED_EDGE ( 'NONE', *, *, #2883, .F. ) ;
#20191 = DIRECTION ( 'NONE',  ( -0.000000000000000000, -0.000000000000000000, -1.000000000000000000 ) ) ;
#20192 = AXIS2_PLACEMENT_3D ( 'NONE', #18571, #2618, #9044 ) ;
#20193 = AXIS2_PLACEMENT_3D ( 'NONE', #15568, #7783, #6062 ) ;
#20194 = ORIENTED_EDGE ( 'NONE', *, *, #220, .T. ) ;
#20195 = ORIENTED_EDGE ( 'NONE', *, *, #4033, .F. ) ;
#20196 = ORIENTED_EDGE ( 'NONE', *, *, #19551, .F. ) ;
#20197 = DIRECTION ( 'NONE',  ( 1.000000000000000000, 0.000000000000000000, 0.000000000000000000 ) ) ;
#20198 = CARTESIAN_POINT ( 'NONE',  ( 60.22232964560483737, 7.948937137877944537, 293.5832628385307999 ) ) ;
#20199 = VERTEX_POINT ( 'NONE', #16497 ) ;
#20200 = DIRECTION ( 'NONE',  ( 0.000000000000000000, 0.000000000000000000, 1.000000000000000000 ) ) ;
#20201 = DIRECTION ( 'NONE',  ( -0.6692498792541753394, -0.7430374143461900838, 0.000000000000000000 ) ) ;
#20202 = AXIS2_PLACEMENT_3D ( 'NONE', #4481, #10712, #16966 ) ;
#20203 = ORIENTED_EDGE ( 'NONE', *, *, #6134, .F. ) ;
#20204 = CARTESIAN_POINT ( 'NONE',  ( -96.45829176898665480, 93.78223209612394839, -27.30616533434335480 ) ) ;
#20205 = VECTOR ( 'NONE', #5396, 1000.000000000000000 ) ;
#20206 = DIRECTION ( 'NONE',  ( -1.000000000000000000, 0.000000000000000000, 0.000000000000000000 ) ) ;
#20207 = CYLINDRICAL_SURFACE ( 'NONE', #19275, 127.4413876050234649 ) ;
#20208 = LINE ( 'NONE', #1002, #14399 ) ;
#20209 = DIRECTION ( 'NONE',  ( -0.9511061040868804550, -0.3088643371590125697, 0.000000000000000000 ) ) ;
#20210 = LINE ( 'NONE', #3138, #13966 ) ;
#20211 = DIRECTION ( 'NONE',  ( 0.000000000000000000, 1.000000000000000000, 0.000000000000000000 ) ) ;
#20212 = VERTEX_POINT ( 'NONE', #19464 ) ;
#20213 = VERTEX_POINT ( 'NONE', #16590 ) ;
#20214 = ORIENTED_EDGE ( 'NONE', *, *, #6635, .F. ) ;
#20215 = AXIS2_PLACEMENT_3D ( 'NONE', #17097, #19851, #3086 ) ;
#20216 = VECTOR ( 'NONE', #15713, 1000.000000000000000 ) ;
#20217 = VECTOR ( 'NONE', #7221, 1000.000000000000000 ) ;
#20218 = ORIENTED_EDGE ( 'NONE', *, *, #15775, .F. ) ;
#20219 = EDGE_CURVE ( 'NONE', #1302, #3145, #17833, .T. ) ;
#20220 = FACE_OUTER_BOUND ( 'NONE', #12032, .T. ) ;
#20221 = AXIS2_PLACEMENT_3D ( 'NONE', #8433, #662, #13119 ) ;
#20222 = ORIENTED_EDGE ( 'NONE', *, *, #10036, .T. ) ;
#20223 = CARTESIAN_POINT ( 'NONE',  ( -85.53020504959707182, -140.9188050298390067, 60.00000000000000000 ) ) ;
#20224 = FACE_BOUND ( 'NONE', #15129, .T. ) ;
#20225 = CARTESIAN_POINT ( 'NONE',  ( -71.18887634719365565, -147.8252249328922687, 49.99999999999999289 ) ) ;
#20226 = DIRECTION ( 'NONE',  ( -1.000000000000000000, 0.000000000000000000, 0.000000000000000000 ) ) ;
#20227 = VERTEX_POINT ( 'NONE', #10240 ) ;
#20228 = FACE_OUTER_BOUND ( 'NONE', #17716, .T. ) ;
#20229 = DIRECTION ( 'NONE',  ( 0.000000000000000000, 0.000000000000000000, 1.000000000000000000 ) ) ;
#20230 = ORIENTED_EDGE ( 'NONE', *, *, #12630, .T. ) ;
#20231 =( BOUNDED_SURFACE ( )  B_SPLINE_SURFACE ( 3, 2, ( 
 ( #20162, #4512, #17098 ),
 ( #19953, #13917, #4829 ),
 ( #3293, #4410, #18433 ),
 ( #1343, #10637, #14023 ),
 ( #6364, #12582, #4618 ),
 ( #2985, #18845, #10744 ),
 ( #4722, #112, #1447 ),
 ( #12277, #7781, #9321 ),
 ( #10948, #16893, #7883 ),
 ( #5954, #15351, #12173 ),
 ( #17316, #15671, #3087 ),
 ( #2881, #16, #6266 ),
 ( #9528, #1234, #10842 ),
 ( #9213, #7472, #17000 ),
 ( #3189, #13712, #7678 ),
 ( #18531, #12478, #15564 ),
 ( #9426, #9108, #7571 ),
 ( #13814, #20060, #6060 ),
 ( #15457, #1656, #1550 ),
 ( #6163, #12382, #18742 ),
 ( #18643, #8289, #18953 ),
 ( #618, #9824, #9929 ),
 ( #12989, #17617, #5037 ),
 ( #12891, #11154, #19146 ),
 ( #12794, #5137, #17416 ),
 ( #3392, #3593, #314 ),
 ( #4939, #3689, #6671 ),
 ( #5329, #6766, #14229 ) ),
 .UNSPECIFIED., .F., .F., .F. ) 
 B_SPLINE_SURFACE_WITH_KNOTS ( ( 4, 2, 2, 2, 2, 2, 2, 2, 2, 2, 2, 2, 2, 4 ),
 ( 3, 3 ),
 ( 0.01172725363905311943, 0.01619455768277540397, 0.01731138369370597424, 0.01842820970463654451, 0.02066186172649768504, 0.02289551374835882558, 0.02401233975928939585, 0.02512916577021996958, 0.02959646981394225412, 0.03406377385766454213, 0.03629742587952568267, 0.03853107790138682320, 0.04299838194510910427, 0.04746568598883138534 ),
 ( 0.000000000000000000, 1.000000000000000000 ),
 .UNSPECIFIED. ) 
 GEOMETRIC_REPRESENTATION_ITEM ( )  RATIONAL_B_SPLINE_SURFACE ( (
 ( 1.000000000000000000, 0.4759858191164941243, 1.000000000000000000),
 ( 1.000000000000000000, 0.4759956267216851611, 1.000000000000000000),
 ( 1.000000000000000000, 0.4778541562206653492, 1.000000000000000000),
 ( 1.000000000000000000, 0.4823973722703661648, 1.000000000000000000),
 ( 1.000000000000000000, 0.4834178931537515544, 1.000000000000000000),
 ( 1.000000000000000000, 0.4856852555521312120, 1.000000000000000000),
 ( 1.000000000000000000, 0.4869309269815854657, 1.000000000000000000),
 ( 1.000000000000000000, 0.4909487690767815882, 1.000000000000000000),
 ( 1.000000000000000000, 0.4940161083580015822, 1.000000000000000000),
 ( 1.000000000000000000, 0.5008835903390461697, 1.000000000000000000),
 ( 1.000000000000000000, 0.5046839780478526993, 1.000000000000000000),
 ( 1.000000000000000000, 0.5109205925582556151, 1.000000000000000000),
 ( 1.000000000000000000, 0.5130943221001723620, 1.000000000000000000),
 ( 1.000000000000000000, 0.5175691686949387416, 1.000000000000000000),
 ( 1.000000000000000000, 0.5198746620752942027, 1.000000000000000000),
 ( 1.000000000000000000, 0.5317265360217148240, 1.000000000000000000),
 ( 1.000000000000000000, 0.5422380167217139002, 1.000000000000000000),
 ( 1.000000000000000000, 0.5650731438340860224, 1.000000000000000000),
 ( 1.000000000000000000, 0.5770759225151704808, 1.000000000000000000),
 ( 1.000000000000000000, 0.5957780208533433042, 1.000000000000000000),
 ( 1.000000000000000000, 0.6021295156453072561, 1.000000000000000000),
 ( 1.000000000000000000, 0.6150481322455569888, 1.000000000000000000),
 ( 1.000000000000000000, 0.6215784740535582609, 1.000000000000000000),
 ( 1.000000000000000000, 0.6411710492548771123, 1.000000000000000000),
 ( 1.000000000000000000, 0.6543107498257758614, 1.000000000000000000),
 ( 1.000000000000000000, 0.6806663510239792103, 1.000000000000000000),
 ( 1.000000000000000000, 0.6938871677789396619, 1.000000000000000000),
 ( 1.000000000000000000, 0.7071067811865474617, 1.000000000000000000) ) ) 
 REPRESENTATION_ITEM ( '' )  SURFACE ( )  );
#20232 = EDGE_CURVE ( 'NONE', #347, #1021, #2575, .T. ) ;
#20233 = LINE ( 'NONE', #18606, #9690 ) ;
#20234 = CARTESIAN_POINT ( 'NONE',  ( 0.000000000000000000, 0.000000000000000000, 293.5832628385307999 ) ) ;
#20235 = EDGE_CURVE ( 'NONE', #4517, #4430, #16201, .T. ) ;
#20236 = VECTOR ( 'NONE', #8131, 1000.000000000000000 ) ;
#20237 = CONICAL_SURFACE ( 'NONE', #6544, 5.035999999999999588, 0.7853981633974425058 ) ;
#20238 = EDGE_CURVE ( 'NONE', #17480, #9831, #11752, .T. ) ;
#20239 = DIRECTION ( 'NONE',  ( 0.000000000000000000, 0.000000000000000000, 1.000000000000000000 ) ) ;
#20240 = CARTESIAN_POINT ( 'NONE',  ( 57.61823435390807902, 19.23677882349220880, 293.5832628385307999 ) ) ;
#20241 = CARTESIAN_POINT ( 'NONE',  ( 0.000000000000000000, 0.000000000000000000, 248.9926560891072143 ) ) ;
#20242 = DIRECTION ( 'NONE',  ( 0.000000000000000000, 0.000000000000000000, -1.000000000000000000 ) ) ;
#20243 = NEXT_ASSEMBLY_USAGE_OCCURRENCE ( 'NAUO1', ' ', ' ', #19034, #17155, $ ) ;
#20244 = NEXT_ASSEMBLY_USAGE_OCCURRENCE ( 'NAUO2', ' ', ' ', #19034, #8640, $ ) ;
#20245 = NEXT_ASSEMBLY_USAGE_OCCURRENCE ( 'NAUO3', ' ', ' ', #19034, #3275, $ ) ;
#20246 = NEXT_ASSEMBLY_USAGE_OCCURRENCE ( 'NAUO4', ' ', ' ', #19034, #8137, $ ) ;
#20247 = NEXT_ASSEMBLY_USAGE_OCCURRENCE ( 'NAUO5', ' ', ' ', #19034, #3524, $ ) ;
#20248 = NEXT_ASSEMBLY_USAGE_OCCURRENCE ( 'NAUO6', ' ', ' ', #19034, #12261, $ ) ;
#20249 = NEXT_ASSEMBLY_USAGE_OCCURRENCE ( 'NAUO7', ' ', ' ', #19034, #8394, $ ) ;
#20250 = NEXT_ASSEMBLY_USAGE_OCCURRENCE ( 'NAUO8', ' ', ' ', #19034, #8394, $ ) ;
#20251 = NEXT_ASSEMBLY_USAGE_OCCURRENCE ( 'NAUO9', ' ', ' ', #19034, #8394, $ ) ;
#20252 = NEXT_ASSEMBLY_USAGE_OCCURRENCE ( 'NAUO10', ' ', ' ', #19034, #8394, $ ) ;
ENDSEC;
END-ISO-10303-21;
